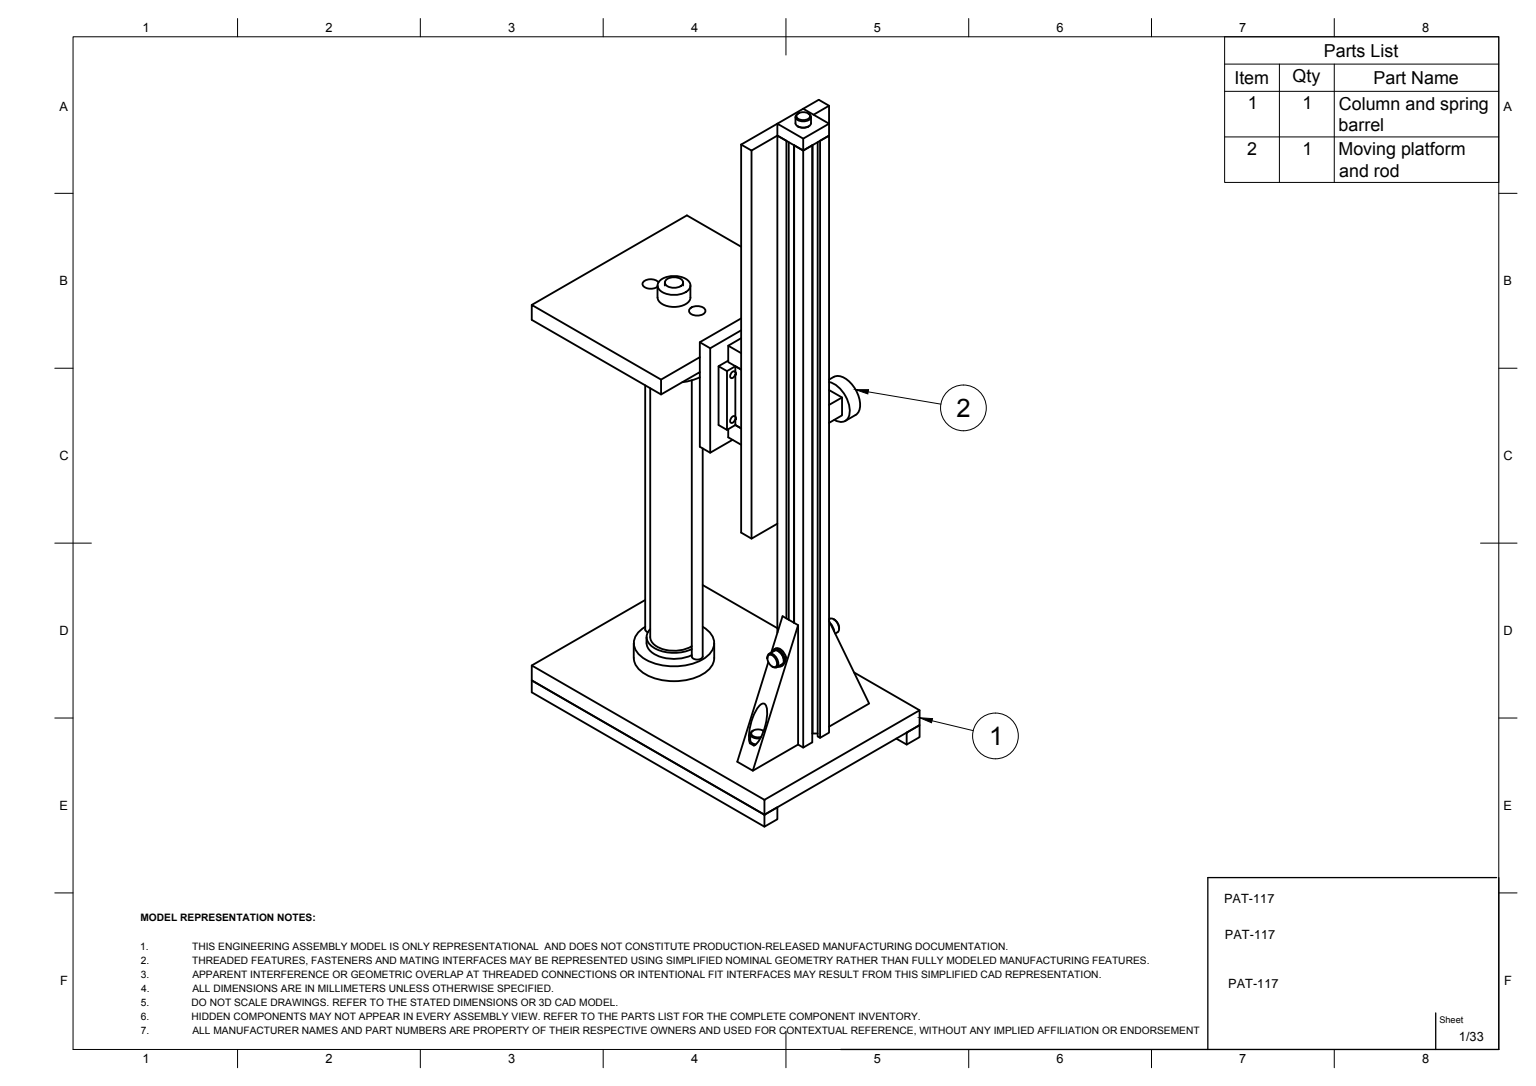
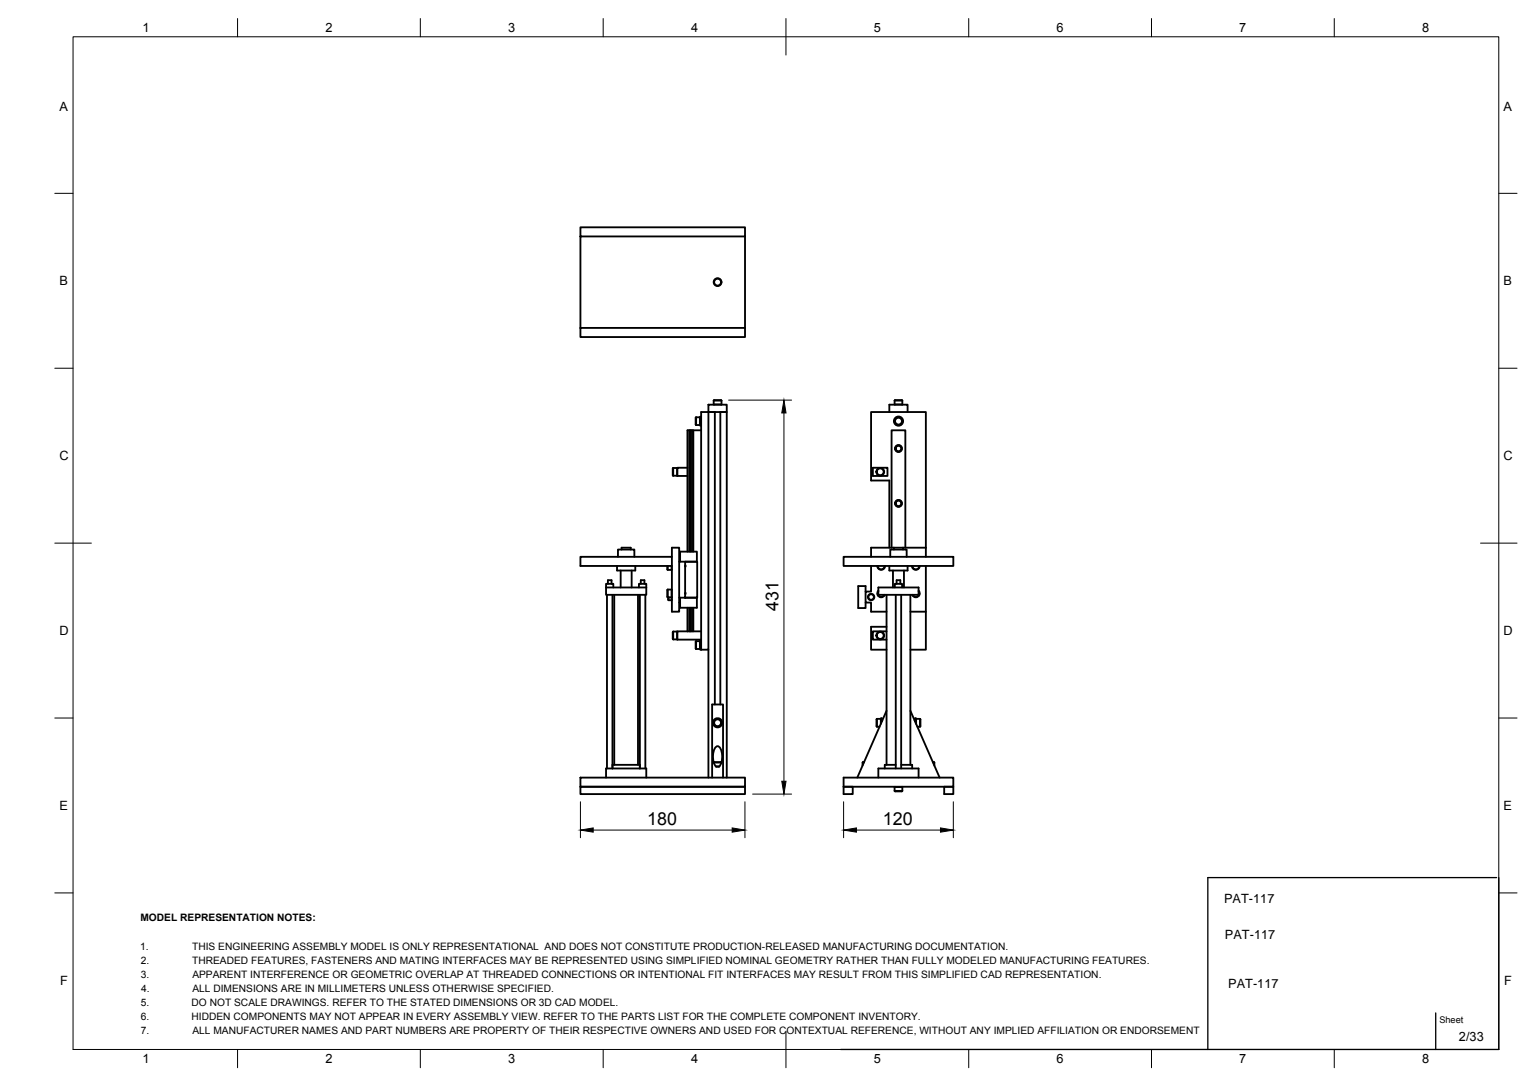
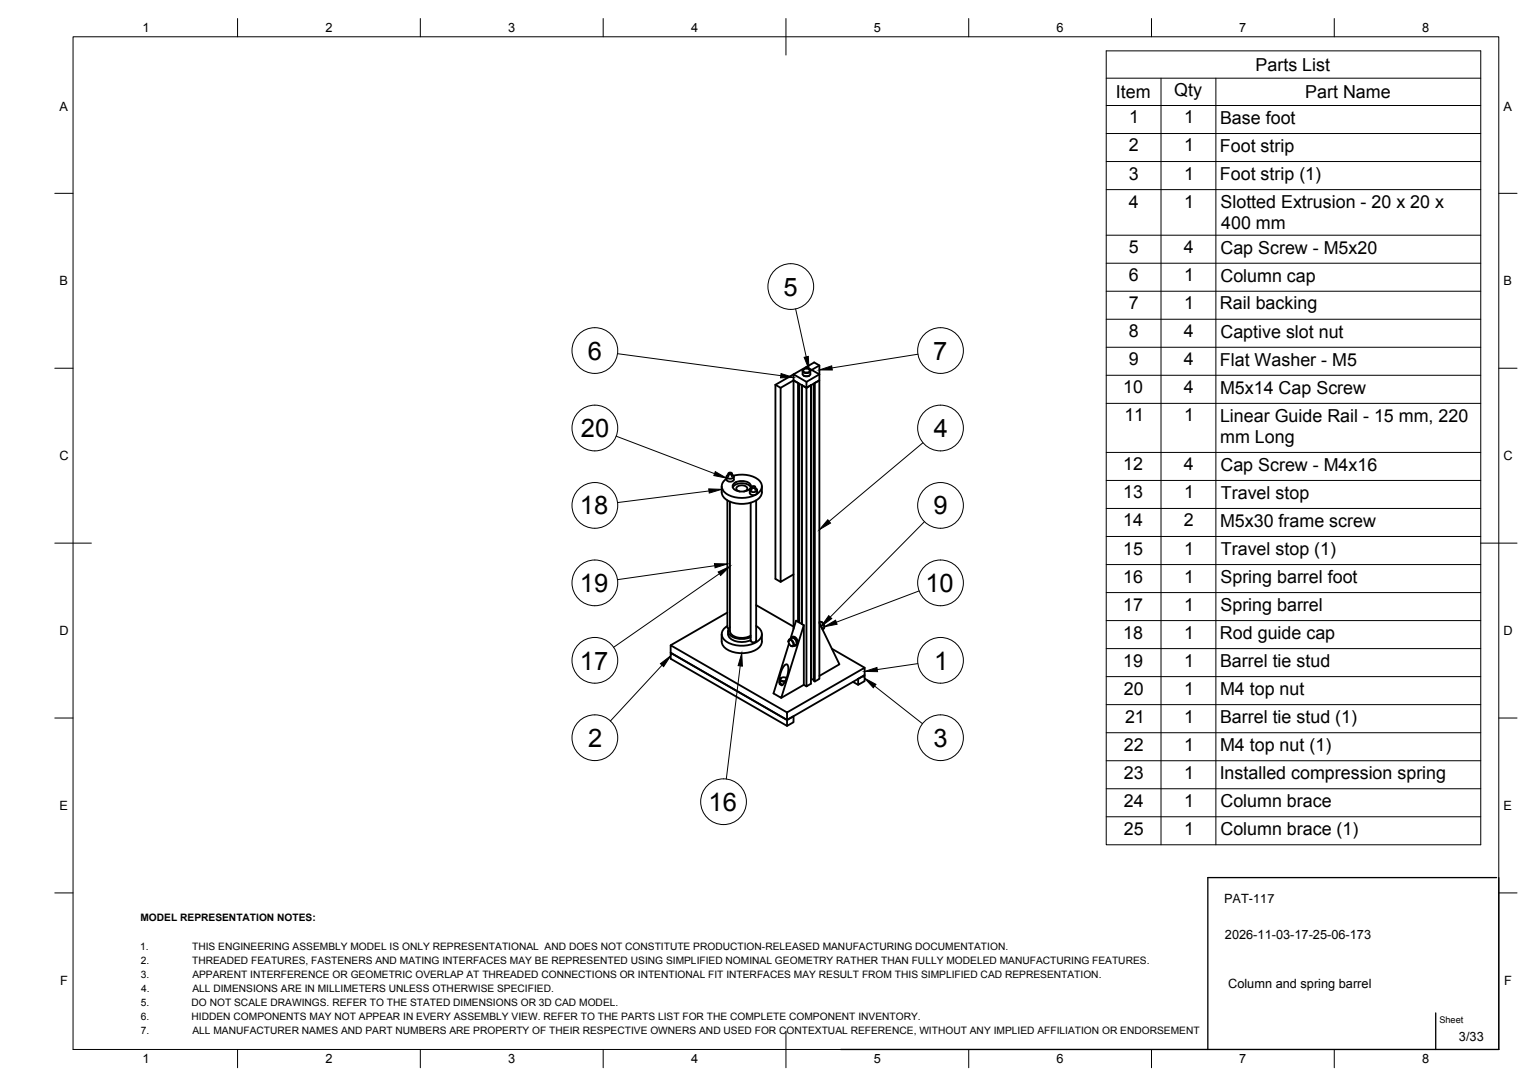
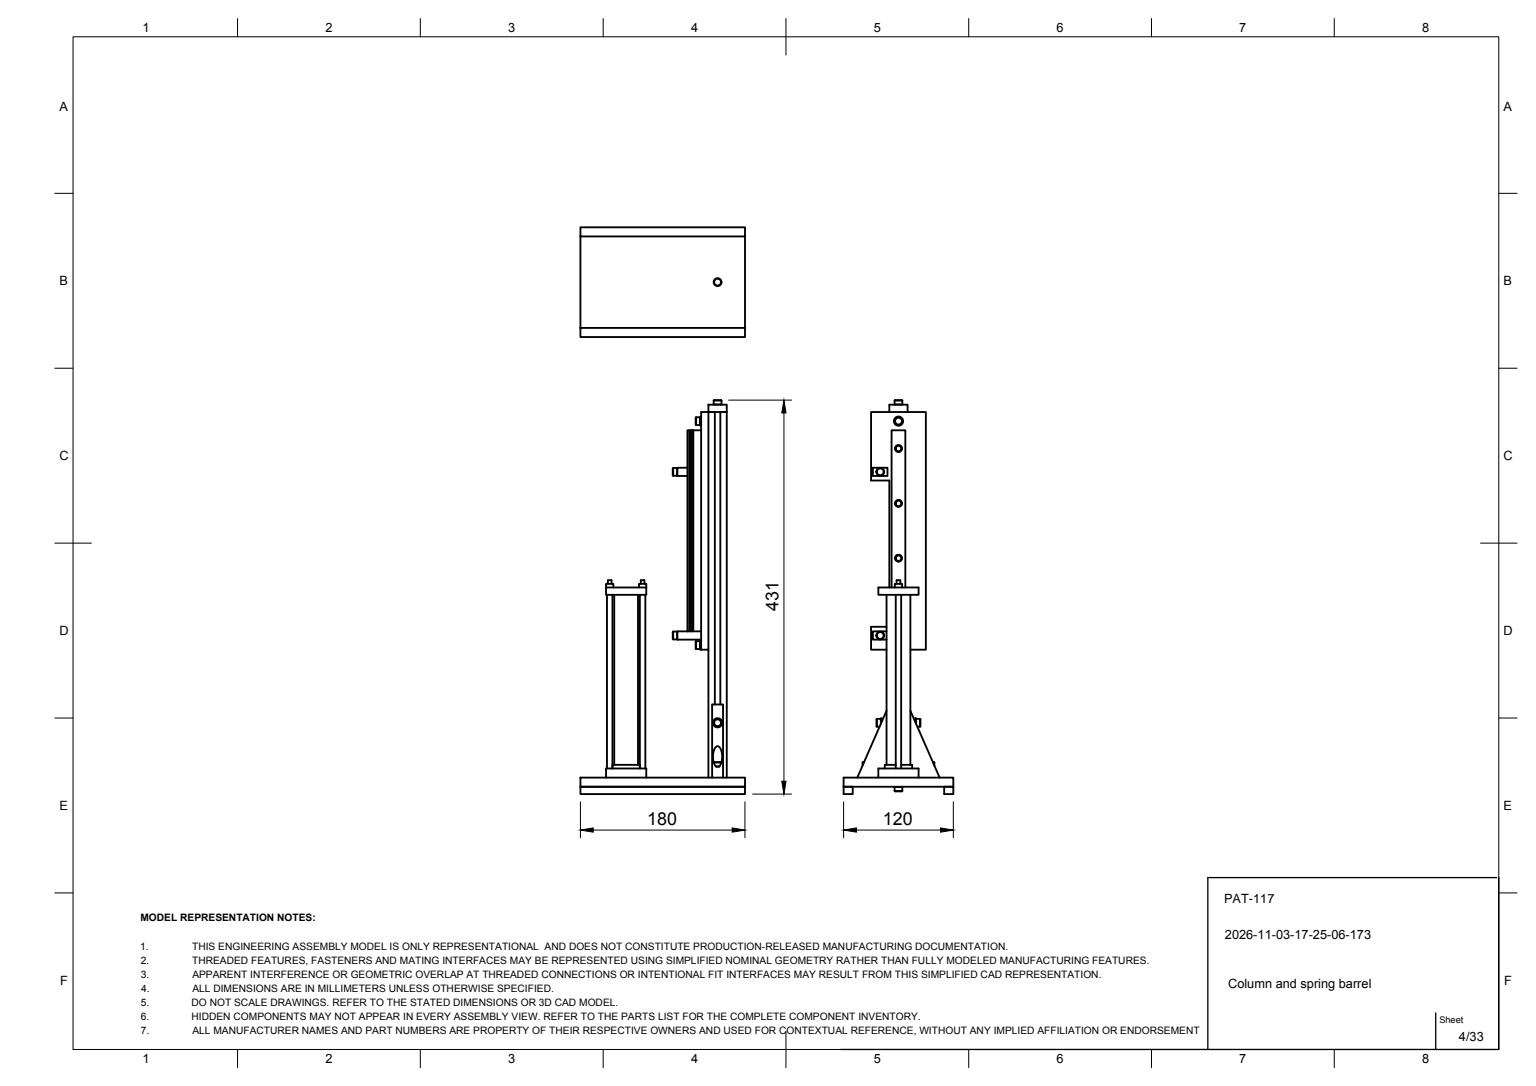
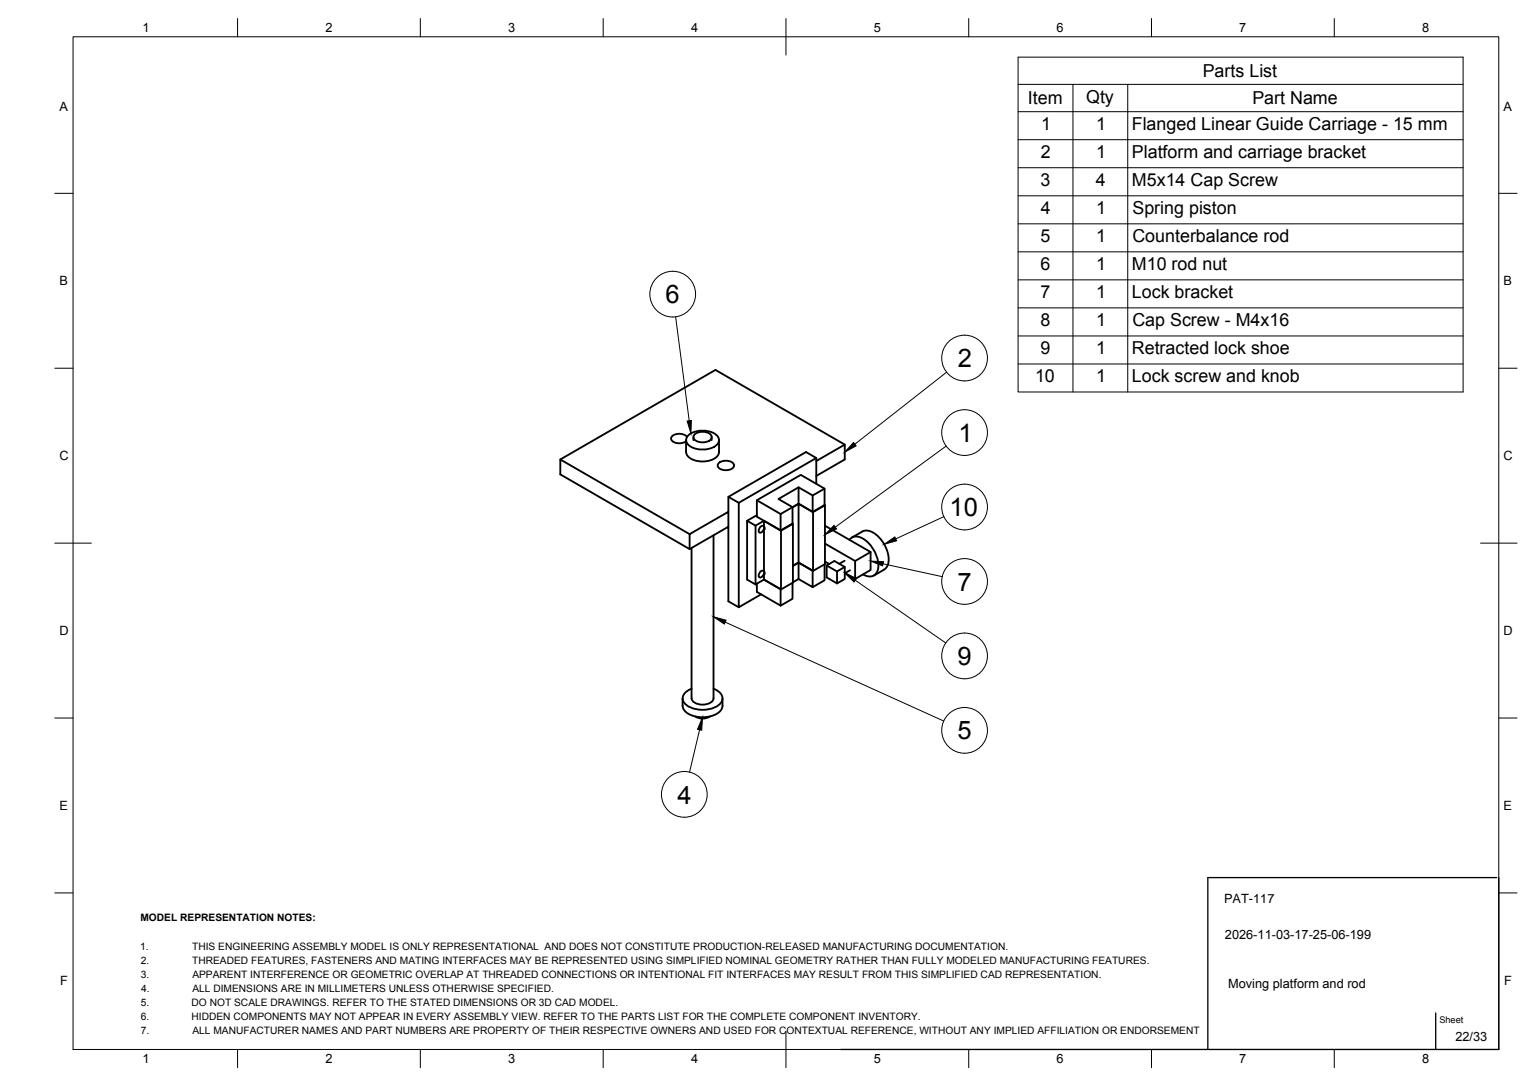
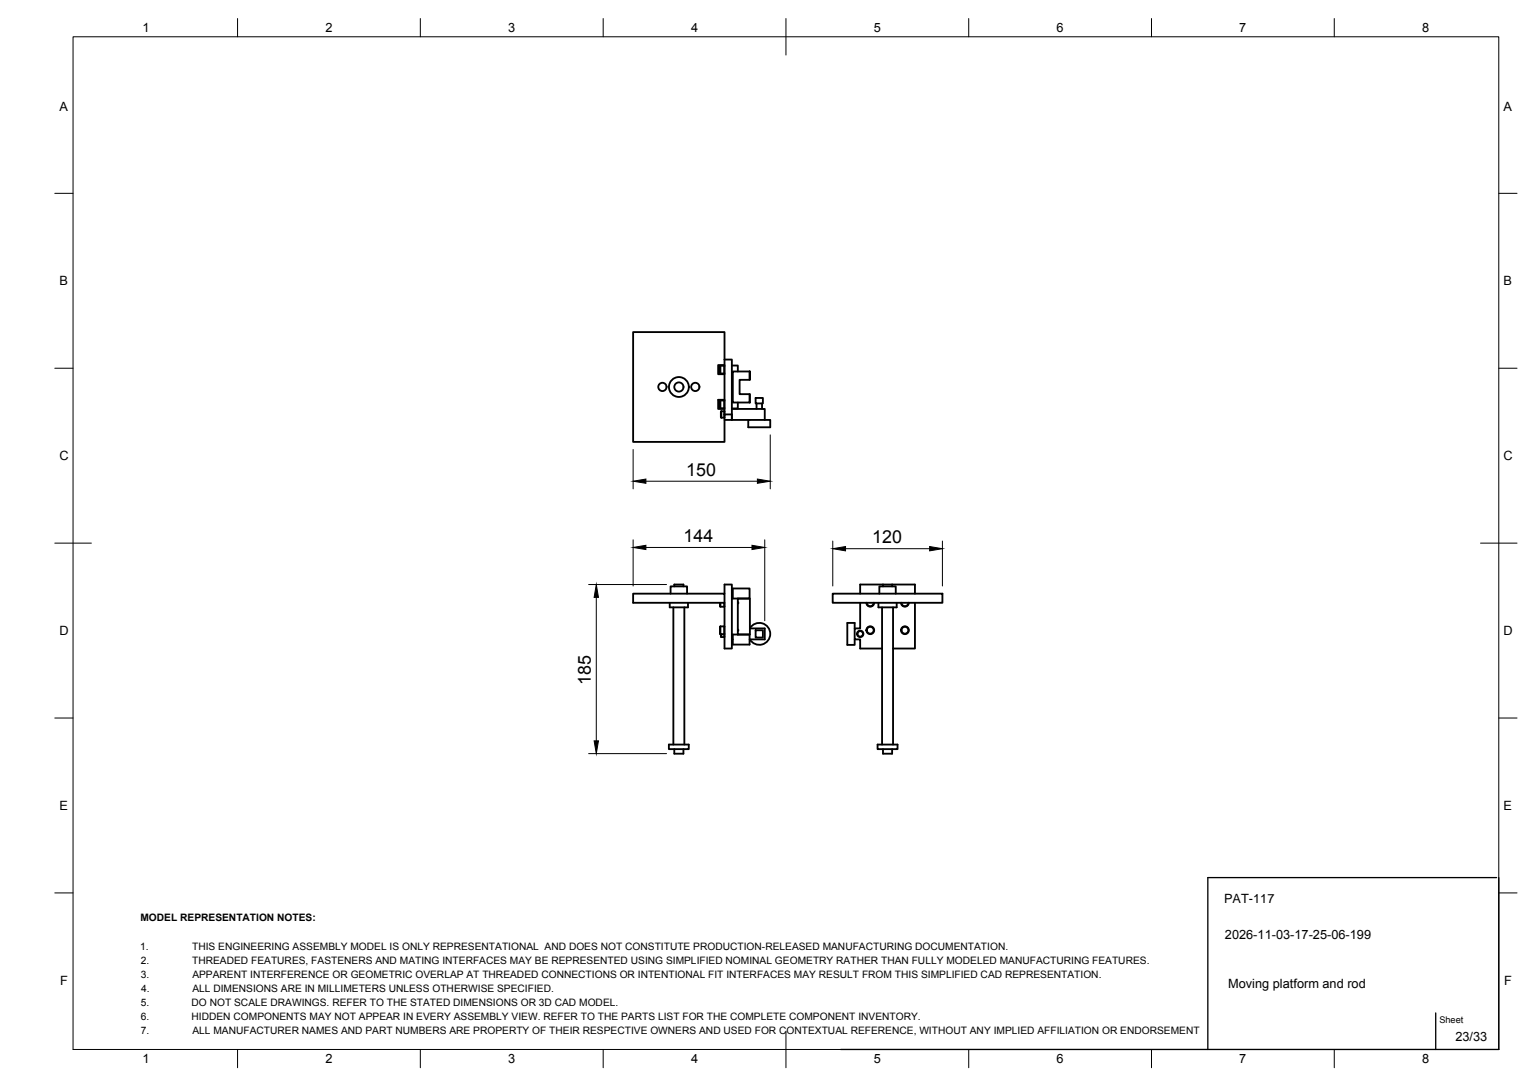
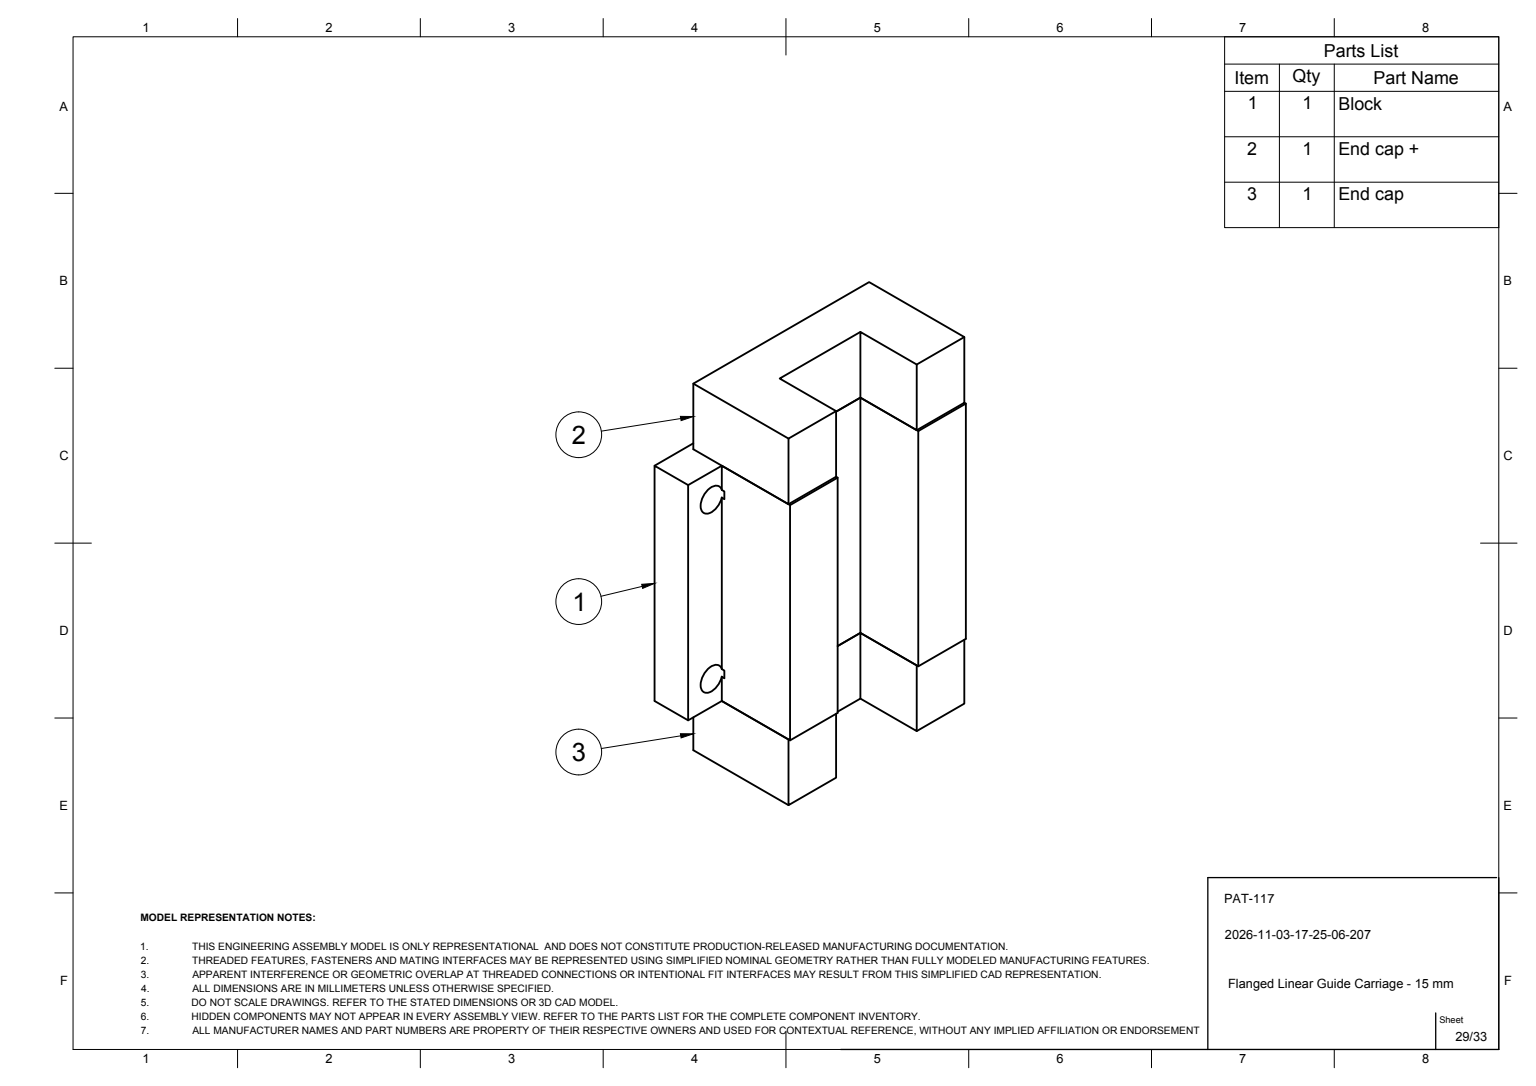
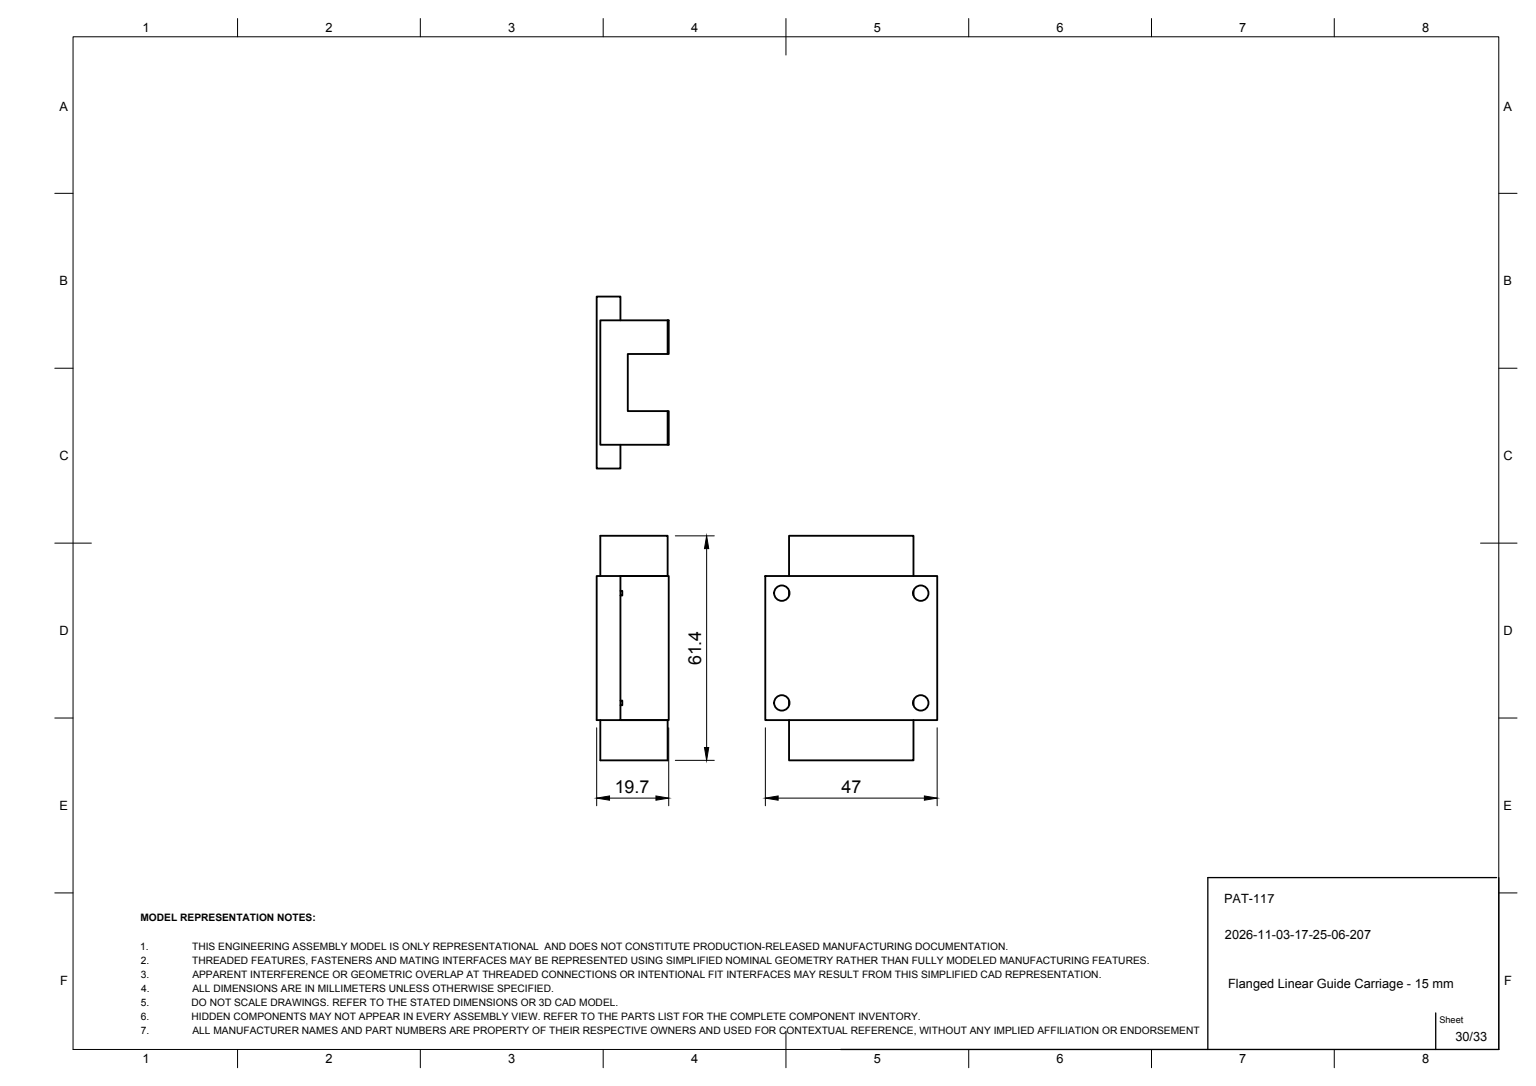
ISO-10303-21;
HEADER;
/* Generated by software containing ST-Developer
 * from STEP Tools, Inc. (www.steptools.com) 
 */

FILE_DESCRIPTION(
/* description */ ('Counterbalanced vertical column'),
/* implementation_level */ '2;1');

FILE_NAME(
/* name */ 'PAT-117',
/* time_stamp */ '2026-10-29T16:47:22-07:00',
/* author */ (''),
/* organization */ (''),
/* preprocessor_version */ 'ST-DEVELOPER v20.2',
/* originating_system */ 'Autodesk Translation Framework v15.17.0.0',
/* authorisation */ '');

FILE_SCHEMA (('AUTOMOTIVE_DESIGN { 1 0 10303 214 3 1 1 }'));
ENDSEC;

DATA;
#10=MECHANICAL_DESIGN_GEOMETRIC_PRESENTATION_REPRESENTATION('',(#350,#351,
#352,#353,#354,#355,#356,#357,#358,#359,#360,#361,#362,#363,#364,#365,#366,
#367,#368,#369,#370,#371,#372,#373,#374,#375,#376,#377,#378,#379,#380,#381,
#382,#383,#384),#15040);
#11=ITEM_DEFINED_TRANSFORMATION($,$,#8051,#8112);
#12=ITEM_DEFINED_TRANSFORMATION($,$,#8090,#8113);
#13=ITEM_DEFINED_TRANSFORMATION($,$,#8101,#8114);
#14=ITEM_DEFINED_TRANSFORMATION($,$,#7500,#8165);
#15=ITEM_DEFINED_TRANSFORMATION($,$,#7526,#8166);
#16=ITEM_DEFINED_TRANSFORMATION($,$,#7533,#8167);
#17=ITEM_DEFINED_TRANSFORMATION($,$,#7540,#8168);
#18=ITEM_DEFINED_TRANSFORMATION($,$,#7550,#8169);
#19=ITEM_DEFINED_TRANSFORMATION($,$,#7585,#8170);
#20=ITEM_DEFINED_TRANSFORMATION($,$,#7595,#8171);
#21=ITEM_DEFINED_TRANSFORMATION($,$,#7605,#8172);
#22=ITEM_DEFINED_TRANSFORMATION($,$,#7625,#8173);
#23=ITEM_DEFINED_TRANSFORMATION($,$,#7634,#8174);
#24=ITEM_DEFINED_TRANSFORMATION($,$,#7657,#8175);
#25=ITEM_DEFINED_TRANSFORMATION($,$,#7671,#8176);
#26=ITEM_DEFINED_TRANSFORMATION($,$,#7680,#8177);
#27=ITEM_DEFINED_TRANSFORMATION($,$,#7694,#8178);
#28=ITEM_DEFINED_TRANSFORMATION($,$,#7703,#8179);
#29=ITEM_DEFINED_TRANSFORMATION($,$,#7708,#8180);
#30=ITEM_DEFINED_TRANSFORMATION($,$,#7730,#8181);
#31=ITEM_DEFINED_TRANSFORMATION($,$,#7752,#8182);
#32=ITEM_DEFINED_TRANSFORMATION($,$,#7873,#8183);
#33=ITEM_DEFINED_TRANSFORMATION($,$,#7873,#8184);
#34=ITEM_DEFINED_TRANSFORMATION($,$,#7899,#8185);
#35=ITEM_DEFINED_TRANSFORMATION($,$,#7920,#8186);
#36=ITEM_DEFINED_TRANSFORMATION($,$,#8115,#8187);
#37=ITEM_DEFINED_TRANSFORMATION($,$,#7899,#8188);
#38=ITEM_DEFINED_TRANSFORMATION($,$,#7920,#8189);
#39=ITEM_DEFINED_TRANSFORMATION($,$,#8115,#8190);
#40=ITEM_DEFINED_TRANSFORMATION($,$,#7802,#8191);
#41=ITEM_DEFINED_TRANSFORMATION($,$,#8139,#8192);
#42=ITEM_DEFINED_TRANSFORMATION($,$,#8139,#8193);
#43=ITEM_DEFINED_TRANSFORMATION($,$,#8139,#8194);
#44=ITEM_DEFINED_TRANSFORMATION($,$,#8139,#8195);
#45=ITEM_DEFINED_TRANSFORMATION($,$,#7845,#8196);
#46=ITEM_DEFINED_TRANSFORMATION($,$,#7845,#8197);
#47=ITEM_DEFINED_TRANSFORMATION($,$,#7873,#8198);
#48=ITEM_DEFINED_TRANSFORMATION($,$,#7899,#8199);
#49=ITEM_DEFINED_TRANSFORMATION($,$,#7920,#8200);
#50=ITEM_DEFINED_TRANSFORMATION($,$,#8115,#8201);
#51=ITEM_DEFINED_TRANSFORMATION($,$,#7873,#8202);
#52=ITEM_DEFINED_TRANSFORMATION($,$,#7899,#8203);
#53=ITEM_DEFINED_TRANSFORMATION($,$,#7920,#8204);
#54=ITEM_DEFINED_TRANSFORMATION($,$,#8115,#8205);
#55=ITEM_DEFINED_TRANSFORMATION($,$,#7932,#8206);
#56=ITEM_DEFINED_TRANSFORMATION($,$,#7983,#8207);
#57=ITEM_DEFINED_TRANSFORMATION($,$,#7992,#8208);
#58=ITEM_DEFINED_TRANSFORMATION($,$,#8010,#8209);
#59=ITEM_DEFINED_TRANSFORMATION($,$,#8019,#8210);
#60=ITEM_DEFINED_TRANSFORMATION($,$,#8033,#8211);
#61=ITEM_DEFINED_TRANSFORMATION($,$,#8040,#8212);
#62=ITEM_DEFINED_TRANSFORMATION($,$,#8050,#8213);
#63=ITEM_DEFINED_TRANSFORMATION($,$,#8115,#8214);
#64=ITEM_DEFINED_TRANSFORMATION($,$,#8115,#8215);
#65=ITEM_DEFINED_TRANSFORMATION($,$,#8115,#8216);
#66=ITEM_DEFINED_TRANSFORMATION($,$,#8115,#8217);
#67=ITEM_DEFINED_TRANSFORMATION($,$,#8139,#8218);
#68=ITEM_DEFINED_TRANSFORMATION($,$,#7499,#8219);
#69=ITEM_DEFINED_TRANSFORMATION($,$,#7931,#8220);
#70=(
REPRESENTATION_RELATIONSHIP($,$,#15216,#15215)
REPRESENTATION_RELATIONSHIP_WITH_TRANSFORMATION(#11)
SHAPE_REPRESENTATION_RELATIONSHIP()
);
#71=(
REPRESENTATION_RELATIONSHIP($,$,#15217,#15215)
REPRESENTATION_RELATIONSHIP_WITH_TRANSFORMATION(#12)
SHAPE_REPRESENTATION_RELATIONSHIP()
);
#72=(
REPRESENTATION_RELATIONSHIP($,$,#15218,#15215)
REPRESENTATION_RELATIONSHIP_WITH_TRANSFORMATION(#13)
SHAPE_REPRESENTATION_RELATIONSHIP()
);
#73=(
REPRESENTATION_RELATIONSHIP($,$,#15184,#15183)
REPRESENTATION_RELATIONSHIP_WITH_TRANSFORMATION(#14)
SHAPE_REPRESENTATION_RELATIONSHIP()
);
#74=(
REPRESENTATION_RELATIONSHIP($,$,#15185,#15183)
REPRESENTATION_RELATIONSHIP_WITH_TRANSFORMATION(#15)
SHAPE_REPRESENTATION_RELATIONSHIP()
);
#75=(
REPRESENTATION_RELATIONSHIP($,$,#15186,#15183)
REPRESENTATION_RELATIONSHIP_WITH_TRANSFORMATION(#16)
SHAPE_REPRESENTATION_RELATIONSHIP()
);
#76=(
REPRESENTATION_RELATIONSHIP($,$,#15187,#15183)
REPRESENTATION_RELATIONSHIP_WITH_TRANSFORMATION(#17)
SHAPE_REPRESENTATION_RELATIONSHIP()
);
#77=(
REPRESENTATION_RELATIONSHIP($,$,#15188,#15183)
REPRESENTATION_RELATIONSHIP_WITH_TRANSFORMATION(#18)
SHAPE_REPRESENTATION_RELATIONSHIP()
);
#78=(
REPRESENTATION_RELATIONSHIP($,$,#15189,#15183)
REPRESENTATION_RELATIONSHIP_WITH_TRANSFORMATION(#19)
SHAPE_REPRESENTATION_RELATIONSHIP()
);
#79=(
REPRESENTATION_RELATIONSHIP($,$,#15190,#15183)
REPRESENTATION_RELATIONSHIP_WITH_TRANSFORMATION(#20)
SHAPE_REPRESENTATION_RELATIONSHIP()
);
#80=(
REPRESENTATION_RELATIONSHIP($,$,#15191,#15183)
REPRESENTATION_RELATIONSHIP_WITH_TRANSFORMATION(#21)
SHAPE_REPRESENTATION_RELATIONSHIP()
);
#81=(
REPRESENTATION_RELATIONSHIP($,$,#15192,#15183)
REPRESENTATION_RELATIONSHIP_WITH_TRANSFORMATION(#22)
SHAPE_REPRESENTATION_RELATIONSHIP()
);
#82=(
REPRESENTATION_RELATIONSHIP($,$,#15193,#15183)
REPRESENTATION_RELATIONSHIP_WITH_TRANSFORMATION(#23)
SHAPE_REPRESENTATION_RELATIONSHIP()
);
#83=(
REPRESENTATION_RELATIONSHIP($,$,#15194,#15183)
REPRESENTATION_RELATIONSHIP_WITH_TRANSFORMATION(#24)
SHAPE_REPRESENTATION_RELATIONSHIP()
);
#84=(
REPRESENTATION_RELATIONSHIP($,$,#15195,#15183)
REPRESENTATION_RELATIONSHIP_WITH_TRANSFORMATION(#25)
SHAPE_REPRESENTATION_RELATIONSHIP()
);
#85=(
REPRESENTATION_RELATIONSHIP($,$,#15196,#15183)
REPRESENTATION_RELATIONSHIP_WITH_TRANSFORMATION(#26)
SHAPE_REPRESENTATION_RELATIONSHIP()
);
#86=(
REPRESENTATION_RELATIONSHIP($,$,#15197,#15183)
REPRESENTATION_RELATIONSHIP_WITH_TRANSFORMATION(#27)
SHAPE_REPRESENTATION_RELATIONSHIP()
);
#87=(
REPRESENTATION_RELATIONSHIP($,$,#15198,#15183)
REPRESENTATION_RELATIONSHIP_WITH_TRANSFORMATION(#28)
SHAPE_REPRESENTATION_RELATIONSHIP()
);
#88=(
REPRESENTATION_RELATIONSHIP($,$,#15199,#15183)
REPRESENTATION_RELATIONSHIP_WITH_TRANSFORMATION(#29)
SHAPE_REPRESENTATION_RELATIONSHIP()
);
#89=(
REPRESENTATION_RELATIONSHIP($,$,#15200,#15183)
REPRESENTATION_RELATIONSHIP_WITH_TRANSFORMATION(#30)
SHAPE_REPRESENTATION_RELATIONSHIP()
);
#90=(
REPRESENTATION_RELATIONSHIP($,$,#15201,#15183)
REPRESENTATION_RELATIONSHIP_WITH_TRANSFORMATION(#31)
SHAPE_REPRESENTATION_RELATIONSHIP()
);
#91=(
REPRESENTATION_RELATIONSHIP($,$,#15204,#15183)
REPRESENTATION_RELATIONSHIP_WITH_TRANSFORMATION(#32)
SHAPE_REPRESENTATION_RELATIONSHIP()
);
#92=(
REPRESENTATION_RELATIONSHIP($,$,#15204,#15183)
REPRESENTATION_RELATIONSHIP_WITH_TRANSFORMATION(#33)
SHAPE_REPRESENTATION_RELATIONSHIP()
);
#93=(
REPRESENTATION_RELATIONSHIP($,$,#15205,#15183)
REPRESENTATION_RELATIONSHIP_WITH_TRANSFORMATION(#34)
SHAPE_REPRESENTATION_RELATIONSHIP()
);
#94=(
REPRESENTATION_RELATIONSHIP($,$,#15206,#15183)
REPRESENTATION_RELATIONSHIP_WITH_TRANSFORMATION(#35)
SHAPE_REPRESENTATION_RELATIONSHIP()
);
#95=(
REPRESENTATION_RELATIONSHIP($,$,#15219,#15183)
REPRESENTATION_RELATIONSHIP_WITH_TRANSFORMATION(#36)
SHAPE_REPRESENTATION_RELATIONSHIP()
);
#96=(
REPRESENTATION_RELATIONSHIP($,$,#15205,#15183)
REPRESENTATION_RELATIONSHIP_WITH_TRANSFORMATION(#37)
SHAPE_REPRESENTATION_RELATIONSHIP()
);
#97=(
REPRESENTATION_RELATIONSHIP($,$,#15206,#15183)
REPRESENTATION_RELATIONSHIP_WITH_TRANSFORMATION(#38)
SHAPE_REPRESENTATION_RELATIONSHIP()
);
#98=(
REPRESENTATION_RELATIONSHIP($,$,#15219,#15183)
REPRESENTATION_RELATIONSHIP_WITH_TRANSFORMATION(#39)
SHAPE_REPRESENTATION_RELATIONSHIP()
);
#99=(
REPRESENTATION_RELATIONSHIP($,$,#15202,#15183)
REPRESENTATION_RELATIONSHIP_WITH_TRANSFORMATION(#40)
SHAPE_REPRESENTATION_RELATIONSHIP()
);
#100=(
REPRESENTATION_RELATIONSHIP($,$,#15220,#15183)
REPRESENTATION_RELATIONSHIP_WITH_TRANSFORMATION(#41)
SHAPE_REPRESENTATION_RELATIONSHIP()
);
#101=(
REPRESENTATION_RELATIONSHIP($,$,#15220,#15183)
REPRESENTATION_RELATIONSHIP_WITH_TRANSFORMATION(#42)
SHAPE_REPRESENTATION_RELATIONSHIP()
);
#102=(
REPRESENTATION_RELATIONSHIP($,$,#15220,#15183)
REPRESENTATION_RELATIONSHIP_WITH_TRANSFORMATION(#43)
SHAPE_REPRESENTATION_RELATIONSHIP()
);
#103=(
REPRESENTATION_RELATIONSHIP($,$,#15220,#15183)
REPRESENTATION_RELATIONSHIP_WITH_TRANSFORMATION(#44)
SHAPE_REPRESENTATION_RELATIONSHIP()
);
#104=(
REPRESENTATION_RELATIONSHIP($,$,#15203,#15183)
REPRESENTATION_RELATIONSHIP_WITH_TRANSFORMATION(#45)
SHAPE_REPRESENTATION_RELATIONSHIP()
);
#105=(
REPRESENTATION_RELATIONSHIP($,$,#15203,#15183)
REPRESENTATION_RELATIONSHIP_WITH_TRANSFORMATION(#46)
SHAPE_REPRESENTATION_RELATIONSHIP()
);
#106=(
REPRESENTATION_RELATIONSHIP($,$,#15204,#15183)
REPRESENTATION_RELATIONSHIP_WITH_TRANSFORMATION(#47)
SHAPE_REPRESENTATION_RELATIONSHIP()
);
#107=(
REPRESENTATION_RELATIONSHIP($,$,#15205,#15183)
REPRESENTATION_RELATIONSHIP_WITH_TRANSFORMATION(#48)
SHAPE_REPRESENTATION_RELATIONSHIP()
);
#108=(
REPRESENTATION_RELATIONSHIP($,$,#15206,#15183)
REPRESENTATION_RELATIONSHIP_WITH_TRANSFORMATION(#49)
SHAPE_REPRESENTATION_RELATIONSHIP()
);
#109=(
REPRESENTATION_RELATIONSHIP($,$,#15219,#15183)
REPRESENTATION_RELATIONSHIP_WITH_TRANSFORMATION(#50)
SHAPE_REPRESENTATION_RELATIONSHIP()
);
#110=(
REPRESENTATION_RELATIONSHIP($,$,#15204,#15183)
REPRESENTATION_RELATIONSHIP_WITH_TRANSFORMATION(#51)
SHAPE_REPRESENTATION_RELATIONSHIP()
);
#111=(
REPRESENTATION_RELATIONSHIP($,$,#15205,#15183)
REPRESENTATION_RELATIONSHIP_WITH_TRANSFORMATION(#52)
SHAPE_REPRESENTATION_RELATIONSHIP()
);
#112=(
REPRESENTATION_RELATIONSHIP($,$,#15206,#15183)
REPRESENTATION_RELATIONSHIP_WITH_TRANSFORMATION(#53)
SHAPE_REPRESENTATION_RELATIONSHIP()
);
#113=(
REPRESENTATION_RELATIONSHIP($,$,#15219,#15183)
REPRESENTATION_RELATIONSHIP_WITH_TRANSFORMATION(#54)
SHAPE_REPRESENTATION_RELATIONSHIP()
);
#114=(
REPRESENTATION_RELATIONSHIP($,$,#15208,#15207)
REPRESENTATION_RELATIONSHIP_WITH_TRANSFORMATION(#55)
SHAPE_REPRESENTATION_RELATIONSHIP()
);
#115=(
REPRESENTATION_RELATIONSHIP($,$,#15209,#15207)
REPRESENTATION_RELATIONSHIP_WITH_TRANSFORMATION(#56)
SHAPE_REPRESENTATION_RELATIONSHIP()
);
#116=(
REPRESENTATION_RELATIONSHIP($,$,#15210,#15207)
REPRESENTATION_RELATIONSHIP_WITH_TRANSFORMATION(#57)
SHAPE_REPRESENTATION_RELATIONSHIP()
);
#117=(
REPRESENTATION_RELATIONSHIP($,$,#15211,#15207)
REPRESENTATION_RELATIONSHIP_WITH_TRANSFORMATION(#58)
SHAPE_REPRESENTATION_RELATIONSHIP()
);
#118=(
REPRESENTATION_RELATIONSHIP($,$,#15212,#15207)
REPRESENTATION_RELATIONSHIP_WITH_TRANSFORMATION(#59)
SHAPE_REPRESENTATION_RELATIONSHIP()
);
#119=(
REPRESENTATION_RELATIONSHIP($,$,#15213,#15207)
REPRESENTATION_RELATIONSHIP_WITH_TRANSFORMATION(#60)
SHAPE_REPRESENTATION_RELATIONSHIP()
);
#120=(
REPRESENTATION_RELATIONSHIP($,$,#15214,#15207)
REPRESENTATION_RELATIONSHIP_WITH_TRANSFORMATION(#61)
SHAPE_REPRESENTATION_RELATIONSHIP()
);
#121=(
REPRESENTATION_RELATIONSHIP($,$,#15215,#15207)
REPRESENTATION_RELATIONSHIP_WITH_TRANSFORMATION(#62)
SHAPE_REPRESENTATION_RELATIONSHIP()
);
#122=(
REPRESENTATION_RELATIONSHIP($,$,#15219,#15207)
REPRESENTATION_RELATIONSHIP_WITH_TRANSFORMATION(#63)
SHAPE_REPRESENTATION_RELATIONSHIP()
);
#123=(
REPRESENTATION_RELATIONSHIP($,$,#15219,#15207)
REPRESENTATION_RELATIONSHIP_WITH_TRANSFORMATION(#64)
SHAPE_REPRESENTATION_RELATIONSHIP()
);
#124=(
REPRESENTATION_RELATIONSHIP($,$,#15219,#15207)
REPRESENTATION_RELATIONSHIP_WITH_TRANSFORMATION(#65)
SHAPE_REPRESENTATION_RELATIONSHIP()
);
#125=(
REPRESENTATION_RELATIONSHIP($,$,#15219,#15207)
REPRESENTATION_RELATIONSHIP_WITH_TRANSFORMATION(#66)
SHAPE_REPRESENTATION_RELATIONSHIP()
);
#126=(
REPRESENTATION_RELATIONSHIP($,$,#15220,#15207)
REPRESENTATION_RELATIONSHIP_WITH_TRANSFORMATION(#67)
SHAPE_REPRESENTATION_RELATIONSHIP()
);
#127=(
REPRESENTATION_RELATIONSHIP($,$,#15183,#15182)
REPRESENTATION_RELATIONSHIP_WITH_TRANSFORMATION(#68)
SHAPE_REPRESENTATION_RELATIONSHIP()
);
#128=(
REPRESENTATION_RELATIONSHIP($,$,#15207,#15182)
REPRESENTATION_RELATIONSHIP_WITH_TRANSFORMATION(#69)
SHAPE_REPRESENTATION_RELATIONSHIP()
);
#129=CONTEXT_DEPENDENT_SHAPE_REPRESENTATION(#70,#15121);
#130=CONTEXT_DEPENDENT_SHAPE_REPRESENTATION(#71,#15122);
#131=CONTEXT_DEPENDENT_SHAPE_REPRESENTATION(#72,#15123);
#132=CONTEXT_DEPENDENT_SHAPE_REPRESENTATION(#73,#15126);
#133=CONTEXT_DEPENDENT_SHAPE_REPRESENTATION(#74,#15127);
#134=CONTEXT_DEPENDENT_SHAPE_REPRESENTATION(#75,#15128);
#135=CONTEXT_DEPENDENT_SHAPE_REPRESENTATION(#76,#15129);
#136=CONTEXT_DEPENDENT_SHAPE_REPRESENTATION(#77,#15130);
#137=CONTEXT_DEPENDENT_SHAPE_REPRESENTATION(#78,#15131);
#138=CONTEXT_DEPENDENT_SHAPE_REPRESENTATION(#79,#15132);
#139=CONTEXT_DEPENDENT_SHAPE_REPRESENTATION(#80,#15133);
#140=CONTEXT_DEPENDENT_SHAPE_REPRESENTATION(#81,#15134);
#141=CONTEXT_DEPENDENT_SHAPE_REPRESENTATION(#82,#15135);
#142=CONTEXT_DEPENDENT_SHAPE_REPRESENTATION(#83,#15136);
#143=CONTEXT_DEPENDENT_SHAPE_REPRESENTATION(#84,#15137);
#144=CONTEXT_DEPENDENT_SHAPE_REPRESENTATION(#85,#15138);
#145=CONTEXT_DEPENDENT_SHAPE_REPRESENTATION(#86,#15139);
#146=CONTEXT_DEPENDENT_SHAPE_REPRESENTATION(#87,#15140);
#147=CONTEXT_DEPENDENT_SHAPE_REPRESENTATION(#88,#15141);
#148=CONTEXT_DEPENDENT_SHAPE_REPRESENTATION(#89,#15142);
#149=CONTEXT_DEPENDENT_SHAPE_REPRESENTATION(#90,#15143);
#150=CONTEXT_DEPENDENT_SHAPE_REPRESENTATION(#91,#15144);
#151=CONTEXT_DEPENDENT_SHAPE_REPRESENTATION(#92,#15145);
#152=CONTEXT_DEPENDENT_SHAPE_REPRESENTATION(#93,#15146);
#153=CONTEXT_DEPENDENT_SHAPE_REPRESENTATION(#94,#15147);
#154=CONTEXT_DEPENDENT_SHAPE_REPRESENTATION(#95,#15148);
#155=CONTEXT_DEPENDENT_SHAPE_REPRESENTATION(#96,#15149);
#156=CONTEXT_DEPENDENT_SHAPE_REPRESENTATION(#97,#15150);
#157=CONTEXT_DEPENDENT_SHAPE_REPRESENTATION(#98,#15151);
#158=CONTEXT_DEPENDENT_SHAPE_REPRESENTATION(#99,#15152);
#159=CONTEXT_DEPENDENT_SHAPE_REPRESENTATION(#100,#15153);
#160=CONTEXT_DEPENDENT_SHAPE_REPRESENTATION(#101,#15154);
#161=CONTEXT_DEPENDENT_SHAPE_REPRESENTATION(#102,#15155);
#162=CONTEXT_DEPENDENT_SHAPE_REPRESENTATION(#103,#15156);
#163=CONTEXT_DEPENDENT_SHAPE_REPRESENTATION(#104,#15157);
#164=CONTEXT_DEPENDENT_SHAPE_REPRESENTATION(#105,#15158);
#165=CONTEXT_DEPENDENT_SHAPE_REPRESENTATION(#106,#15159);
#166=CONTEXT_DEPENDENT_SHAPE_REPRESENTATION(#107,#15160);
#167=CONTEXT_DEPENDENT_SHAPE_REPRESENTATION(#108,#15161);
#168=CONTEXT_DEPENDENT_SHAPE_REPRESENTATION(#109,#15162);
#169=CONTEXT_DEPENDENT_SHAPE_REPRESENTATION(#110,#15163);
#170=CONTEXT_DEPENDENT_SHAPE_REPRESENTATION(#111,#15164);
#171=CONTEXT_DEPENDENT_SHAPE_REPRESENTATION(#112,#15165);
#172=CONTEXT_DEPENDENT_SHAPE_REPRESENTATION(#113,#15166);
#173=CONTEXT_DEPENDENT_SHAPE_REPRESENTATION(#114,#15167);
#174=CONTEXT_DEPENDENT_SHAPE_REPRESENTATION(#115,#15168);
#175=CONTEXT_DEPENDENT_SHAPE_REPRESENTATION(#116,#15169);
#176=CONTEXT_DEPENDENT_SHAPE_REPRESENTATION(#117,#15170);
#177=CONTEXT_DEPENDENT_SHAPE_REPRESENTATION(#118,#15171);
#178=CONTEXT_DEPENDENT_SHAPE_REPRESENTATION(#119,#15172);
#179=CONTEXT_DEPENDENT_SHAPE_REPRESENTATION(#120,#15173);
#180=CONTEXT_DEPENDENT_SHAPE_REPRESENTATION(#121,#15174);
#181=CONTEXT_DEPENDENT_SHAPE_REPRESENTATION(#122,#15175);
#182=CONTEXT_DEPENDENT_SHAPE_REPRESENTATION(#123,#15176);
#183=CONTEXT_DEPENDENT_SHAPE_REPRESENTATION(#124,#15177);
#184=CONTEXT_DEPENDENT_SHAPE_REPRESENTATION(#125,#15178);
#185=CONTEXT_DEPENDENT_SHAPE_REPRESENTATION(#126,#15179);
#186=CONTEXT_DEPENDENT_SHAPE_REPRESENTATION(#127,#15180);
#187=CONTEXT_DEPENDENT_SHAPE_REPRESENTATION(#128,#15181);
#188=NEXT_ASSEMBLY_USAGE_OCCURRENCE('Block:1','Block:1','Block:1',#15255,
#15256,'Block:1');
#189=NEXT_ASSEMBLY_USAGE_OCCURRENCE('End cap +:1','End cap +:1',
'End cap +:1',#15255,#15257,'End cap +:1');
#190=NEXT_ASSEMBLY_USAGE_OCCURRENCE('End cap:1','End cap:1','End cap:1',
#15255,#15258,'End cap:1');
#191=NEXT_ASSEMBLY_USAGE_OCCURRENCE('Base foot:1','Base foot:1',
'Base foot:1',#15223,#15224,'Base foot:1');
#192=NEXT_ASSEMBLY_USAGE_OCCURRENCE('Foot strip:1','Foot strip:1',
'Foot strip:1',#15223,#15225,'Foot strip:1');
#193=NEXT_ASSEMBLY_USAGE_OCCURRENCE('Foot strip (1):1',
'Foot strip (1):1','Foot strip (1):1',#15223,#15226,'Foot strip (1):1');
#194=NEXT_ASSEMBLY_USAGE_OCCURRENCE('Column cap:1','Column cap:1',
'Column cap:1',#15223,#15227,'Column cap:1');
#195=NEXT_ASSEMBLY_USAGE_OCCURRENCE('Rail backing:1','Rail backing:1',
'Rail backing:1',#15223,#15228,'Rail backing:1');
#196=NEXT_ASSEMBLY_USAGE_OCCURRENCE('Travel stop:1','Travel stop:1',
'Travel stop:1',#15223,#15229,'Travel stop:1');
#197=NEXT_ASSEMBLY_USAGE_OCCURRENCE('Travel stop (1):1',
'Travel stop (1):1','Travel stop (1):1',#15223,#15230,
'Travel stop (1):1');
#198=NEXT_ASSEMBLY_USAGE_OCCURRENCE('Spring barrel foot:1',
'Spring barrel foot:1','Spring barrel foot:1',#15223,#15231,
'Spring barrel foot:1');
#199=NEXT_ASSEMBLY_USAGE_OCCURRENCE('Spring barrel:1','Spring barrel:1',
'Spring barrel:1',#15223,#15232,'Spring barrel:1');
#200=NEXT_ASSEMBLY_USAGE_OCCURRENCE('Rod guide cap:1','Rod guide cap:1',
'Rod guide cap:1',#15223,#15233,'Rod guide cap:1');
#201=NEXT_ASSEMBLY_USAGE_OCCURRENCE('Barrel tie stud:1',
'Barrel tie stud:1','Barrel tie stud:1',#15223,#15234,
'Barrel tie stud:1');
#202=NEXT_ASSEMBLY_USAGE_OCCURRENCE('M4 top nut:1','M4 top nut:1',
'M4 top nut:1',#15223,#15235,'M4 top nut:1');
#203=NEXT_ASSEMBLY_USAGE_OCCURRENCE('Barrel tie stud (1):1',
'Barrel tie stud (1):1','Barrel tie stud (1):1',#15223,#15236,
'Barrel tie stud (1):1');
#204=NEXT_ASSEMBLY_USAGE_OCCURRENCE('M4 top nut (1):1',
'M4 top nut (1):1','M4 top nut (1):1',#15223,#15237,'M4 top nut (1):1');
#205=NEXT_ASSEMBLY_USAGE_OCCURRENCE('Installed compression spring:1',
'Installed compression spring:1','Installed compression spring:1',#15223,
#15238,'Installed compression spring:1');
#206=NEXT_ASSEMBLY_USAGE_OCCURRENCE('Column brace:1','Column brace:1',
'Column brace:1',#15223,#15239,'Column brace:1');
#207=NEXT_ASSEMBLY_USAGE_OCCURRENCE('Column brace (1):1',
'Column brace (1):1','Column brace (1):1',#15223,#15240,
'Column brace (1):1');
#208=NEXT_ASSEMBLY_USAGE_OCCURRENCE(
'Slotted Extrusion - 20 x 20 x 400 mm:2',
'Slotted Extrusion - 20 x 20 x 400 mm:2',
'Slotted Extrusion - 20 x 20 x 400 mm:2',#15223,#15241,
'Slotted Extrusion - 20 x 20 x 400 mm:2');
#209=NEXT_ASSEMBLY_USAGE_OCCURRENCE('Cap Screw - M5x20:2',
'Cap Screw - M5x20:2','Cap Screw - M5x20:2',#15223,#15244,
'Cap Screw - M5x20:2');
#210=NEXT_ASSEMBLY_USAGE_OCCURRENCE('Cap Screw - M5x20:3',
'Cap Screw - M5x20:3','Cap Screw - M5x20:3',#15223,#15244,
'Cap Screw - M5x20:3');
#211=NEXT_ASSEMBLY_USAGE_OCCURRENCE('Captive slot nut:2',
'Captive slot nut:2','Captive slot nut:2',#15223,#15245,
'Captive slot nut:2');
#212=NEXT_ASSEMBLY_USAGE_OCCURRENCE('Flat Washer - M5:2',
'Flat Washer - M5:2','Flat Washer - M5:2',#15223,#15246,
'Flat Washer - M5:2');
#213=NEXT_ASSEMBLY_USAGE_OCCURRENCE('M5x14 Cap Screw:2',
'M5x14 Cap Screw:2','M5x14 Cap Screw:2',#15223,#15259,
'M5x14 Cap Screw:2');
#214=NEXT_ASSEMBLY_USAGE_OCCURRENCE('Captive slot nut:3',
'Captive slot nut:3','Captive slot nut:3',#15223,#15245,
'Captive slot nut:3');
#215=NEXT_ASSEMBLY_USAGE_OCCURRENCE('Flat Washer - M5:3',
'Flat Washer - M5:3','Flat Washer - M5:3',#15223,#15246,
'Flat Washer - M5:3');
#216=NEXT_ASSEMBLY_USAGE_OCCURRENCE('M5x14 Cap Screw:3',
'M5x14 Cap Screw:3','M5x14 Cap Screw:3',#15223,#15259,
'M5x14 Cap Screw:3');
#217=NEXT_ASSEMBLY_USAGE_OCCURRENCE(
'Linear Guide Rail - 15 mm, 220 mm Long:2',
'Linear Guide Rail - 15 mm, 220 mm Long:2',
'Linear Guide Rail - 15 mm, 220 mm Long:2',#15223,#15242,
'Linear Guide Rail - 15 mm, 220 mm Long:2');
#218=NEXT_ASSEMBLY_USAGE_OCCURRENCE('Cap Screw - M4x16:2',
'Cap Screw - M4x16:2','Cap Screw - M4x16:2',#15223,#15260,
'Cap Screw - M4x16:2');
#219=NEXT_ASSEMBLY_USAGE_OCCURRENCE('Cap Screw - M4x16:3',
'Cap Screw - M4x16:3','Cap Screw - M4x16:3',#15223,#15260,
'Cap Screw - M4x16:3');
#220=NEXT_ASSEMBLY_USAGE_OCCURRENCE('Cap Screw - M4x16:4',
'Cap Screw - M4x16:4','Cap Screw - M4x16:4',#15223,#15260,
'Cap Screw - M4x16:4');
#221=NEXT_ASSEMBLY_USAGE_OCCURRENCE('Cap Screw - M4x16:5',
'Cap Screw - M4x16:5','Cap Screw - M4x16:5',#15223,#15260,
'Cap Screw - M4x16:5');
#222=NEXT_ASSEMBLY_USAGE_OCCURRENCE('M5x30 frame screw:2',
'M5x30 frame screw:2','M5x30 frame screw:2',#15223,#15243,
'M5x30 frame screw:2');
#223=NEXT_ASSEMBLY_USAGE_OCCURRENCE('M5x30 frame screw:3',
'M5x30 frame screw:3','M5x30 frame screw:3',#15223,#15243,
'M5x30 frame screw:3');
#224=NEXT_ASSEMBLY_USAGE_OCCURRENCE('Cap Screw - M5x20:4',
'Cap Screw - M5x20:4','Cap Screw - M5x20:4',#15223,#15244,
'Cap Screw - M5x20:4');
#225=NEXT_ASSEMBLY_USAGE_OCCURRENCE('Captive slot nut:4',
'Captive slot nut:4','Captive slot nut:4',#15223,#15245,
'Captive slot nut:4');
#226=NEXT_ASSEMBLY_USAGE_OCCURRENCE('Flat Washer - M5:4',
'Flat Washer - M5:4','Flat Washer - M5:4',#15223,#15246,
'Flat Washer - M5:4');
#227=NEXT_ASSEMBLY_USAGE_OCCURRENCE('M5x14 Cap Screw:8',
'M5x14 Cap Screw:8','M5x14 Cap Screw:8',#15223,#15259,
'M5x14 Cap Screw:8');
#228=NEXT_ASSEMBLY_USAGE_OCCURRENCE('Cap Screw - M5x20:5',
'Cap Screw - M5x20:5','Cap Screw - M5x20:5',#15223,#15244,
'Cap Screw - M5x20:5');
#229=NEXT_ASSEMBLY_USAGE_OCCURRENCE('Captive slot nut:5',
'Captive slot nut:5','Captive slot nut:5',#15223,#15245,
'Captive slot nut:5');
#230=NEXT_ASSEMBLY_USAGE_OCCURRENCE('Flat Washer - M5:5',
'Flat Washer - M5:5','Flat Washer - M5:5',#15223,#15246,
'Flat Washer - M5:5');
#231=NEXT_ASSEMBLY_USAGE_OCCURRENCE('M5x14 Cap Screw:9',
'M5x14 Cap Screw:9','M5x14 Cap Screw:9',#15223,#15259,
'M5x14 Cap Screw:9');
#232=NEXT_ASSEMBLY_USAGE_OCCURRENCE('Platform and carriage bracket:1',
'Platform and carriage bracket:1','Platform and carriage bracket:1',#15247,
#15248,'Platform and carriage bracket:1');
#233=NEXT_ASSEMBLY_USAGE_OCCURRENCE('Spring piston:1','Spring piston:1',
'Spring piston:1',#15247,#15249,'Spring piston:1');
#234=NEXT_ASSEMBLY_USAGE_OCCURRENCE('Counterbalance rod:1',
'Counterbalance rod:1','Counterbalance rod:1',#15247,#15250,
'Counterbalance rod:1');
#235=NEXT_ASSEMBLY_USAGE_OCCURRENCE('M10 rod nut:1','M10 rod nut:1',
'M10 rod nut:1',#15247,#15251,'M10 rod nut:1');
#236=NEXT_ASSEMBLY_USAGE_OCCURRENCE('Lock bracket:1','Lock bracket:1',
'Lock bracket:1',#15247,#15252,'Lock bracket:1');
#237=NEXT_ASSEMBLY_USAGE_OCCURRENCE('Retracted lock shoe:1',
'Retracted lock shoe:1','Retracted lock shoe:1',#15247,#15253,
'Retracted lock shoe:1');
#238=NEXT_ASSEMBLY_USAGE_OCCURRENCE('Lock screw and knob:1',
'Lock screw and knob:1','Lock screw and knob:1',#15247,#15254,
'Lock screw and knob:1');
#239=NEXT_ASSEMBLY_USAGE_OCCURRENCE(
'Flanged Linear Guide Carriage - 15 mm:2',
'Flanged Linear Guide Carriage - 15 mm:2',
'Flanged Linear Guide Carriage - 15 mm:2',#15247,#15255,
'Flanged Linear Guide Carriage - 15 mm:2');
#240=NEXT_ASSEMBLY_USAGE_OCCURRENCE('M5x14 Cap Screw:4',
'M5x14 Cap Screw:4','M5x14 Cap Screw:4',#15247,#15259,
'M5x14 Cap Screw:4');
#241=NEXT_ASSEMBLY_USAGE_OCCURRENCE('M5x14 Cap Screw:5',
'M5x14 Cap Screw:5','M5x14 Cap Screw:5',#15247,#15259,
'M5x14 Cap Screw:5');
#242=NEXT_ASSEMBLY_USAGE_OCCURRENCE('M5x14 Cap Screw:6',
'M5x14 Cap Screw:6','M5x14 Cap Screw:6',#15247,#15259,
'M5x14 Cap Screw:6');
#243=NEXT_ASSEMBLY_USAGE_OCCURRENCE('M5x14 Cap Screw:7',
'M5x14 Cap Screw:7','M5x14 Cap Screw:7',#15247,#15259,
'M5x14 Cap Screw:7');
#244=NEXT_ASSEMBLY_USAGE_OCCURRENCE('Cap Screw - M4x16:6',
'Cap Screw - M4x16:6','Cap Screw - M4x16:6',#15247,#15260,
'Cap Screw - M4x16:6');
#245=NEXT_ASSEMBLY_USAGE_OCCURRENCE('Column and spring barrel:1',
'Column and spring barrel:1','Column and spring barrel:1',#15222,#15223,
'Column and spring barrel:1');
#246=NEXT_ASSEMBLY_USAGE_OCCURRENCE('Moving platform and rod:1',
'Moving platform and rod:1','Moving platform and rod:1',#15222,#15247,
'Moving platform and rod:1');
#247=CONICAL_SURFACE('',#7862,0.4,0.785398163397448);
#248=CONICAL_SURFACE('',#7866,0.41,0.785398163397448);
#249=CONICAL_SURFACE('',#7870,0.26,0.463647609000806);
#250=CONICAL_SURFACE('',#7876,0.4,0.785398163397448);
#251=CONICAL_SURFACE('',#7880,0.41,0.785398163397448);
#252=CONICAL_SURFACE('',#7884,0.26,0.463647609000806);
#253=CONICAL_SURFACE('',#7888,0.225,0.785398163397448);
#254=CONICAL_SURFACE('',#7921,0.275,0.785398163397449);
#255=CONICAL_SURFACE('',#8128,0.4,0.785398163397448);
#256=CONICAL_SURFACE('',#8132,0.41,0.785398163397448);
#257=CONICAL_SURFACE('',#8136,0.26,0.463647609000806);
#258=CONICAL_SURFACE('',#8142,0.325,0.785398163397448);
#259=CONICAL_SURFACE('',#8146,0.335,0.785398163397448);
#260=CONICAL_SURFACE('',#8150,0.21,0.463647609000806);
#261=CONICAL_SURFACE('',#8154,0.18,0.785398163397448);
#262=ORIENTED_CLOSED_SHELL('',*,#7092,.F.);
#263=ORIENTED_CLOSED_SHELL('',*,#7095,.F.);
#264=ORIENTED_CLOSED_SHELL('',*,#7108,.F.);
#265=ORIENTED_CLOSED_SHELL('',*,#7111,.F.);
#266=BREP_WITH_VOIDS('Body1',#7093,(#262));
#267=BREP_WITH_VOIDS('Body1',#7094,(#263));
#268=BREP_WITH_VOIDS('Body1',#7109,(#264));
#269=BREP_WITH_VOIDS('Body1',#7110,(#265));
#270=ELLIPSE('',#7710,0.545757787392906,0.5);
#271=ELLIPSE('',#7716,1.24744637118378,0.5);
#272=ELLIPSE('',#7717,0.300166783066098,0.275);
#273=ELLIPSE('',#7732,0.545757787392906,0.5);
#274=ELLIPSE('',#7738,1.24744637118378,0.5);
#275=ELLIPSE('',#7739,0.300166783066098,0.275);
#276=ELLIPSE('',#7910,0.299389011154384,0.2117);
#277=ELLIPSE('',#7914,0.299389011154384,0.2117);
#278=B_SPLINE_CURVE_WITH_KNOTS('',3,(#13224,#13225,#13226,#13227,#13228,
#13229,#13230,#13231,#13232,#13233,#13234,#13235,#13236,#13237,#13238,#13239,
#13240,#13241,#13242,#13243,#13244,#13245,#13246,#13247,#13248,#13249,#13250,
#13251,#13252,#13253,#13254,#13255,#13256,#13257,#13258,#13259,#13260,#13261,
#13262,#13263,#13264,#13265,#13266,#13267,#13268,#13269,#13270,#13271,#13272,
#13273,#13274,#13275,#13276,#13277,#13278,#13279,#13280,#13281,#13282,#13283,
#13284,#13285,#13286,#13287,#13288,#13289,#13290,#13291,#13292,#13293,#13294,
#13295,#13296,#13297,#13298,#13299,#13300,#13301,#13302,#13303,#13304,#13305,
#13306,#13307,#13308,#13309,#13310,#13311,#13312,#13313,#13314,#13315,#13316,
#13317,#13318,#13319,#13320,#13321,#13322,#13323,#13324,#13325,#13326,#13327,
#13328,#13329,#13330,#13331,#13332,#13333,#13334,#13335,#13336,#13337,#13338,
#13339,#13340,#13341,#13342,#13343,#13344,#13345,#13346,#13347,#13348,#13349,
#13350,#13351,#13352,#13353,#13354,#13355,#13356,#13357,#13358,#13359,#13360,
#13361,#13362,#13363,#13364,#13365,#13366,#13367,#13368,#13369,#13370,#13371,
#13372,#13373,#13374,#13375,#13376,#13377,#13378,#13379,#13380,#13381,#13382,
#13383,#13384,#13385,#13386,#13387,#13388,#13389,#13390,#13391,#13392,#13393,
#13394,#13395,#13396,#13397,#13398,#13399,#13400,#13401,#13402,#13403,#13404,
#13405,#13406,#13407,#13408,#13409,#13410,#13411,#13412,#13413,#13414,#13415,
#13416,#13417,#13418,#13419,#13420,#13421,#13422,#13423,#13424,#13425,#13426,
#13427,#13428,#13429,#13430,#13431,#13432,#13433,#13434,#13435,#13436,#13437,
#13438,#13439,#13440,#13441,#13442,#13443,#13444,#13445,#13446,#13447,#13448,
#13449,#13450,#13451,#13452,#13453,#13454,#13455,#13456,#13457,#13458,#13459,
#13460,#13461,#13462,#13463),.UNSPECIFIED.,.F.,.F.,(4,1,1,1,1,1,1,1,1,1,
1,1,1,1,1,1,1,1,1,1,1,1,1,1,1,1,1,1,1,1,1,1,1,1,1,1,1,1,1,1,1,1,1,1,1,1,
1,1,1,1,1,1,1,1,1,1,1,1,1,1,1,1,1,1,1,1,1,1,1,1,1,1,1,1,1,1,1,1,1,1,1,1,
1,1,1,1,1,1,1,1,1,1,1,1,1,1,1,1,1,1,1,1,1,1,1,1,1,1,1,1,1,1,1,1,1,1,1,1,
1,1,1,1,1,1,1,1,1,1,1,1,1,1,1,1,1,1,1,1,1,1,1,1,1,1,1,1,1,1,1,1,1,1,1,1,
1,1,1,1,1,1,1,1,1,1,1,1,1,1,1,1,1,1,1,1,1,1,1,1,1,1,1,1,1,1,1,1,1,1,1,1,
1,1,1,1,1,1,1,1,1,1,1,1,1,1,1,1,1,1,1,1,1,1,1,1,1,1,1,1,1,1,1,1,1,1,1,1,
1,1,1,1,1,1,1,1,1,1,1,4),(0.,0.00446428571428571,0.00892857142857143,0.0133928571428571,
0.0178571428571429,0.0223214285714286,0.0267857142857143,0.03125,0.0357142857142857,
0.0401785714285714,0.0446428571428571,0.0491071428571428,0.0513392857142857,
0.0535714285714286,0.0580357142857143,0.0625,0.0669642857142857,0.0714285714285714,
0.0758928571428571,0.0803571428571428,0.0848214285714286,0.0892857142857143,
0.09375,0.0982142857142857,0.102678571428571,0.107142857142857,0.111607142857143,
0.116071428571429,0.120535714285714,0.125,0.129464285714286,0.133928571428571,
0.136160714285714,0.138392857142857,0.142857142857143,0.146825396825397,
0.150793650793651,0.154761904761905,0.158730158730159,0.162698412698413,
0.166666666666667,0.170634920634921,0.174603174603175,0.17989417989418,
0.185185185185185,0.19047619047619,0.194444444444444,0.198412698412698,
0.202380952380952,0.206349206349206,0.21031746031746,0.214285714285714,
0.218253968253968,0.220238095238095,0.222222222222222,0.226190476190476,
0.23015873015873,0.234126984126984,0.238095238095238,0.241071428571429,
0.244047619047619,0.247023809523809,0.25,0.25297619047619,0.255952380952381,
0.258928571428571,0.261904761904762,0.267857142857143,0.273809523809524,
0.279761904761905,0.285714285714286,0.291666666666667,0.297619047619048,
0.303571428571429,0.30952380952381,0.31547619047619,0.321428571428571,0.327380952380952,
0.333333333333333,0.339285714285714,0.345238095238095,0.351190476190476,
0.357142857142857,0.363095238095238,0.369047619047619,0.375,0.380952380952381,
0.386904761904762,0.392857142857143,0.398809523809524,0.404761904761905,
0.407738095238095,0.410714285714286,0.413690476190476,0.416666666666667,
0.419642857142857,0.422619047619048,0.425595238095238,0.428571428571429,
0.433035714285714,0.4375,0.441964285714286,0.446428571428571,0.450892857142857,
0.455357142857143,0.459821428571429,0.464285714285714,0.46875,0.473214285714286,
0.477678571428571,0.482142857142857,0.486607142857143,0.491071428571429,
0.495535714285714,0.5,0.504464285714286,0.508928571428571,0.513392857142857,
0.517857142857143,0.522321428571428,0.526785714285714,0.53125,0.535714285714286,
0.540178571428571,0.544642857142857,0.549107142857143,0.553571428571429,
0.558035714285714,0.5625,0.566964285714286,0.571428571428571,0.575892857142857,
0.580357142857143,0.584821428571428,0.589285714285714,0.59375,0.598214285714286,
0.602678571428571,0.607142857142857,0.611607142857143,0.616071428571429,
0.620535714285714,0.625,0.627232142857143,0.629464285714286,0.633928571428571,
0.638392857142857,0.642857142857143,0.645833333333333,0.648809523809524,
0.651785714285714,0.654761904761905,0.657738095238095,0.660714285714286,
0.663690476190476,0.666666666666667,0.66765873015873,0.670634920634921,
0.674603174603175,0.678571428571428,0.683035714285714,0.6875,0.691964285714286,
0.696428571428571,0.700892857142857,0.705357142857143,0.709821428571428,
0.714285714285714,0.717261904761905,0.720238095238095,0.723214285714286,
0.726190476190476,0.729166666666667,0.732142857142857,0.735119047619047,
0.738095238095238,0.744047619047619,0.75,0.755952380952381,0.761904761904762,
0.767857142857143,0.773809523809524,0.779761904761905,0.785714285714286,
0.78968253968254,0.793650793650793,0.797619047619047,0.801587301587302,
0.805555555555555,0.809523809523809,0.8125,0.81547619047619,0.818452380952381,
0.821428571428571,0.824404761904762,0.827380952380952,0.833333333333333,
0.836309523809524,0.839285714285714,0.842261904761905,0.845238095238095,
0.848214285714286,0.851190476190476,0.854166666666667,0.857142857142857,
0.861607142857143,0.866071428571429,0.870535714285714,0.875,0.879464285714286,
0.883928571428571,0.888392857142857,0.892857142857143,0.897321428571428,
0.901785714285714,0.90625,0.910714285714286,0.915178571428571,0.919642857142857,
0.924107142857143,0.928571428571429,0.930803571428571,0.933035714285714,
0.9375,0.941964285714286,0.946428571428571,0.950892857142857,0.955357142857143,
0.959821428571429,0.964285714285714,0.96875,0.973214285714286,0.977678571428572,
0.982142857142857,0.986607142857143,0.991071428571429,0.995535714285714,
1.),.UNSPECIFIED.);
#279=B_SPLINE_SURFACE_WITH_KNOTS('',3,3,((#10821,#10822,#10823,#10824,#10825,
#10826,#10827,#10828,#10829,#10830,#10831,#10832,#10833,#10834,#10835,#10836,
#10837,#10838,#10839,#10840,#10841,#10842,#10843,#10844,#10845,#10846,#10847,
#10848,#10849,#10850,#10851,#10852,#10853,#10854,#10855,#10856,#10857,#10858,
#10859,#10860,#10861,#10862,#10863,#10864,#10865,#10866,#10867,#10868,#10869,
#10870,#10871,#10872,#10873,#10874,#10875,#10876,#10877,#10878,#10879,#10880,
#10881,#10882,#10883,#10884,#10885,#10886,#10887,#10888,#10889,#10890,#10891,
#10892,#10893,#10894,#10895,#10896,#10897,#10898,#10899,#10900,#10901,#10902,
#10903,#10904,#10905,#10906,#10907,#10908,#10909,#10910,#10911,#10912,#10913,
#10914,#10915,#10916,#10917,#10918,#10919,#10920,#10921,#10922,#10923,#10924,
#10925,#10926,#10927,#10928,#10929,#10930,#10931,#10932,#10933,#10934,#10935,
#10936,#10937,#10938,#10939,#10940,#10941,#10942,#10943,#10944,#10945,#10946,
#10947,#10948,#10949,#10950,#10951,#10952,#10953,#10954,#10955,#10956,#10957,
#10958,#10959,#10960,#10961,#10962,#10963,#10964,#10965,#10966,#10967,#10968,
#10969,#10970,#10971,#10972,#10973,#10974,#10975,#10976,#10977,#10978,#10979,
#10980,#10981,#10982,#10983,#10984,#10985,#10986,#10987,#10988,#10989,#10990,
#10991,#10992,#10993,#10994,#10995,#10996,#10997,#10998,#10999,#11000,#11001,
#11002,#11003,#11004,#11005,#11006,#11007,#11008,#11009,#11010,#11011,#11012,
#11013,#11014,#11015,#11016,#11017,#11018,#11019,#11020,#11021,#11022,#11023,
#11024,#11025,#11026,#11027,#11028,#11029,#11030,#11031,#11032,#11033,#11034,
#11035,#11036,#11037,#11038,#11039,#11040,#11041,#11042,#11043,#11044,#11045,
#11046,#11047,#11048,#11049,#11050,#11051,#11052,#11053,#11054,#11055,#11056,
#11057,#11058,#11059,#11060),(#11061,#11062,#11063,#11064,#11065,#11066,
#11067,#11068,#11069,#11070,#11071,#11072,#11073,#11074,#11075,#11076,#11077,
#11078,#11079,#11080,#11081,#11082,#11083,#11084,#11085,#11086,#11087,#11088,
#11089,#11090,#11091,#11092,#11093,#11094,#11095,#11096,#11097,#11098,#11099,
#11100,#11101,#11102,#11103,#11104,#11105,#11106,#11107,#11108,#11109,#11110,
#11111,#11112,#11113,#11114,#11115,#11116,#11117,#11118,#11119,#11120,#11121,
#11122,#11123,#11124,#11125,#11126,#11127,#11128,#11129,#11130,#11131,#11132,
#11133,#11134,#11135,#11136,#11137,#11138,#11139,#11140,#11141,#11142,#11143,
#11144,#11145,#11146,#11147,#11148,#11149,#11150,#11151,#11152,#11153,#11154,
#11155,#11156,#11157,#11158,#11159,#11160,#11161,#11162,#11163,#11164,#11165,
#11166,#11167,#11168,#11169,#11170,#11171,#11172,#11173,#11174,#11175,#11176,
#11177,#11178,#11179,#11180,#11181,#11182,#11183,#11184,#11185,#11186,#11187,
#11188,#11189,#11190,#11191,#11192,#11193,#11194,#11195,#11196,#11197,#11198,
#11199,#11200,#11201,#11202,#11203,#11204,#11205,#11206,#11207,#11208,#11209,
#11210,#11211,#11212,#11213,#11214,#11215,#11216,#11217,#11218,#11219,#11220,
#11221,#11222,#11223,#11224,#11225,#11226,#11227,#11228,#11229,#11230,#11231,
#11232,#11233,#11234,#11235,#11236,#11237,#11238,#11239,#11240,#11241,#11242,
#11243,#11244,#11245,#11246,#11247,#11248,#11249,#11250,#11251,#11252,#11253,
#11254,#11255,#11256,#11257,#11258,#11259,#11260,#11261,#11262,#11263,#11264,
#11265,#11266,#11267,#11268,#11269,#11270,#11271,#11272,#11273,#11274,#11275,
#11276,#11277,#11278,#11279,#11280,#11281,#11282,#11283,#11284,#11285,#11286,
#11287,#11288,#11289,#11290,#11291,#11292,#11293,#11294,#11295,#11296,#11297,
#11298,#11299,#11300),(#11301,#11302,#11303,#11304,#11305,#11306,#11307,
#11308,#11309,#11310,#11311,#11312,#11313,#11314,#11315,#11316,#11317,#11318,
#11319,#11320,#11321,#11322,#11323,#11324,#11325,#11326,#11327,#11328,#11329,
#11330,#11331,#11332,#11333,#11334,#11335,#11336,#11337,#11338,#11339,#11340,
#11341,#11342,#11343,#11344,#11345,#11346,#11347,#11348,#11349,#11350,#11351,
#11352,#11353,#11354,#11355,#11356,#11357,#11358,#11359,#11360,#11361,#11362,
#11363,#11364,#11365,#11366,#11367,#11368,#11369,#11370,#11371,#11372,#11373,
#11374,#11375,#11376,#11377,#11378,#11379,#11380,#11381,#11382,#11383,#11384,
#11385,#11386,#11387,#11388,#11389,#11390,#11391,#11392,#11393,#11394,#11395,
#11396,#11397,#11398,#11399,#11400,#11401,#11402,#11403,#11404,#11405,#11406,
#11407,#11408,#11409,#11410,#11411,#11412,#11413,#11414,#11415,#11416,#11417,
#11418,#11419,#11420,#11421,#11422,#11423,#11424,#11425,#11426,#11427,#11428,
#11429,#11430,#11431,#11432,#11433,#11434,#11435,#11436,#11437,#11438,#11439,
#11440,#11441,#11442,#11443,#11444,#11445,#11446,#11447,#11448,#11449,#11450,
#11451,#11452,#11453,#11454,#11455,#11456,#11457,#11458,#11459,#11460,#11461,
#11462,#11463,#11464,#11465,#11466,#11467,#11468,#11469,#11470,#11471,#11472,
#11473,#11474,#11475,#11476,#11477,#11478,#11479,#11480,#11481,#11482,#11483,
#11484,#11485,#11486,#11487,#11488,#11489,#11490,#11491,#11492,#11493,#11494,
#11495,#11496,#11497,#11498,#11499,#11500,#11501,#11502,#11503,#11504,#11505,
#11506,#11507,#11508,#11509,#11510,#11511,#11512,#11513,#11514,#11515,#11516,
#11517,#11518,#11519,#11520,#11521,#11522,#11523,#11524,#11525,#11526,#11527,
#11528,#11529,#11530,#11531,#11532,#11533,#11534,#11535,#11536,#11537,#11538,
#11539,#11540),(#11541,#11542,#11543,#11544,#11545,#11546,#11547,#11548,
#11549,#11550,#11551,#11552,#11553,#11554,#11555,#11556,#11557,#11558,#11559,
#11560,#11561,#11562,#11563,#11564,#11565,#11566,#11567,#11568,#11569,#11570,
#11571,#11572,#11573,#11574,#11575,#11576,#11577,#11578,#11579,#11580,#11581,
#11582,#11583,#11584,#11585,#11586,#11587,#11588,#11589,#11590,#11591,#11592,
#11593,#11594,#11595,#11596,#11597,#11598,#11599,#11600,#11601,#11602,#11603,
#11604,#11605,#11606,#11607,#11608,#11609,#11610,#11611,#11612,#11613,#11614,
#11615,#11616,#11617,#11618,#11619,#11620,#11621,#11622,#11623,#11624,#11625,
#11626,#11627,#11628,#11629,#11630,#11631,#11632,#11633,#11634,#11635,#11636,
#11637,#11638,#11639,#11640,#11641,#11642,#11643,#11644,#11645,#11646,#11647,
#11648,#11649,#11650,#11651,#11652,#11653,#11654,#11655,#11656,#11657,#11658,
#11659,#11660,#11661,#11662,#11663,#11664,#11665,#11666,#11667,#11668,#11669,
#11670,#11671,#11672,#11673,#11674,#11675,#11676,#11677,#11678,#11679,#11680,
#11681,#11682,#11683,#11684,#11685,#11686,#11687,#11688,#11689,#11690,#11691,
#11692,#11693,#11694,#11695,#11696,#11697,#11698,#11699,#11700,#11701,#11702,
#11703,#11704,#11705,#11706,#11707,#11708,#11709,#11710,#11711,#11712,#11713,
#11714,#11715,#11716,#11717,#11718,#11719,#11720,#11721,#11722,#11723,#11724,
#11725,#11726,#11727,#11728,#11729,#11730,#11731,#11732,#11733,#11734,#11735,
#11736,#11737,#11738,#11739,#11740,#11741,#11742,#11743,#11744,#11745,#11746,
#11747,#11748,#11749,#11750,#11751,#11752,#11753,#11754,#11755,#11756,#11757,
#11758,#11759,#11760,#11761,#11762,#11763,#11764,#11765,#11766,#11767,#11768,
#11769,#11770,#11771,#11772,#11773,#11774,#11775,#11776,#11777,#11778,#11779,
#11780),(#11781,#11782,#11783,#11784,#11785,#11786,#11787,#11788,#11789,
#11790,#11791,#11792,#11793,#11794,#11795,#11796,#11797,#11798,#11799,#11800,
#11801,#11802,#11803,#11804,#11805,#11806,#11807,#11808,#11809,#11810,#11811,
#11812,#11813,#11814,#11815,#11816,#11817,#11818,#11819,#11820,#11821,#11822,
#11823,#11824,#11825,#11826,#11827,#11828,#11829,#11830,#11831,#11832,#11833,
#11834,#11835,#11836,#11837,#11838,#11839,#11840,#11841,#11842,#11843,#11844,
#11845,#11846,#11847,#11848,#11849,#11850,#11851,#11852,#11853,#11854,#11855,
#11856,#11857,#11858,#11859,#11860,#11861,#11862,#11863,#11864,#11865,#11866,
#11867,#11868,#11869,#11870,#11871,#11872,#11873,#11874,#11875,#11876,#11877,
#11878,#11879,#11880,#11881,#11882,#11883,#11884,#11885,#11886,#11887,#11888,
#11889,#11890,#11891,#11892,#11893,#11894,#11895,#11896,#11897,#11898,#11899,
#11900,#11901,#11902,#11903,#11904,#11905,#11906,#11907,#11908,#11909,#11910,
#11911,#11912,#11913,#11914,#11915,#11916,#11917,#11918,#11919,#11920,#11921,
#11922,#11923,#11924,#11925,#11926,#11927,#11928,#11929,#11930,#11931,#11932,
#11933,#11934,#11935,#11936,#11937,#11938,#11939,#11940,#11941,#11942,#11943,
#11944,#11945,#11946,#11947,#11948,#11949,#11950,#11951,#11952,#11953,#11954,
#11955,#11956,#11957,#11958,#11959,#11960,#11961,#11962,#11963,#11964,#11965,
#11966,#11967,#11968,#11969,#11970,#11971,#11972,#11973,#11974,#11975,#11976,
#11977,#11978,#11979,#11980,#11981,#11982,#11983,#11984,#11985,#11986,#11987,
#11988,#11989,#11990,#11991,#11992,#11993,#11994,#11995,#11996,#11997,#11998,
#11999,#12000,#12001,#12002,#12003,#12004,#12005,#12006,#12007,#12008,#12009,
#12010,#12011,#12012,#12013,#12014,#12015,#12016,#12017,#12018,#12019,#12020),
(#12021,#12022,#12023,#12024,#12025,#12026,#12027,#12028,#12029,#12030,
#12031,#12032,#12033,#12034,#12035,#12036,#12037,#12038,#12039,#12040,#12041,
#12042,#12043,#12044,#12045,#12046,#12047,#12048,#12049,#12050,#12051,#12052,
#12053,#12054,#12055,#12056,#12057,#12058,#12059,#12060,#12061,#12062,#12063,
#12064,#12065,#12066,#12067,#12068,#12069,#12070,#12071,#12072,#12073,#12074,
#12075,#12076,#12077,#12078,#12079,#12080,#12081,#12082,#12083,#12084,#12085,
#12086,#12087,#12088,#12089,#12090,#12091,#12092,#12093,#12094,#12095,#12096,
#12097,#12098,#12099,#12100,#12101,#12102,#12103,#12104,#12105,#12106,#12107,
#12108,#12109,#12110,#12111,#12112,#12113,#12114,#12115,#12116,#12117,#12118,
#12119,#12120,#12121,#12122,#12123,#12124,#12125,#12126,#12127,#12128,#12129,
#12130,#12131,#12132,#12133,#12134,#12135,#12136,#12137,#12138,#12139,#12140,
#12141,#12142,#12143,#12144,#12145,#12146,#12147,#12148,#12149,#12150,#12151,
#12152,#12153,#12154,#12155,#12156,#12157,#12158,#12159,#12160,#12161,#12162,
#12163,#12164,#12165,#12166,#12167,#12168,#12169,#12170,#12171,#12172,#12173,
#12174,#12175,#12176,#12177,#12178,#12179,#12180,#12181,#12182,#12183,#12184,
#12185,#12186,#12187,#12188,#12189,#12190,#12191,#12192,#12193,#12194,#12195,
#12196,#12197,#12198,#12199,#12200,#12201,#12202,#12203,#12204,#12205,#12206,
#12207,#12208,#12209,#12210,#12211,#12212,#12213,#12214,#12215,#12216,#12217,
#12218,#12219,#12220,#12221,#12222,#12223,#12224,#12225,#12226,#12227,#12228,
#12229,#12230,#12231,#12232,#12233,#12234,#12235,#12236,#12237,#12238,#12239,
#12240,#12241,#12242,#12243,#12244,#12245,#12246,#12247,#12248,#12249,#12250,
#12251,#12252,#12253,#12254,#12255,#12256,#12257,#12258,#12259,#12260),
(#12261,#12262,#12263,#12264,#12265,#12266,#12267,#12268,#12269,#12270,
#12271,#12272,#12273,#12274,#12275,#12276,#12277,#12278,#12279,#12280,#12281,
#12282,#12283,#12284,#12285,#12286,#12287,#12288,#12289,#12290,#12291,#12292,
#12293,#12294,#12295,#12296,#12297,#12298,#12299,#12300,#12301,#12302,#12303,
#12304,#12305,#12306,#12307,#12308,#12309,#12310,#12311,#12312,#12313,#12314,
#12315,#12316,#12317,#12318,#12319,#12320,#12321,#12322,#12323,#12324,#12325,
#12326,#12327,#12328,#12329,#12330,#12331,#12332,#12333,#12334,#12335,#12336,
#12337,#12338,#12339,#12340,#12341,#12342,#12343,#12344,#12345,#12346,#12347,
#12348,#12349,#12350,#12351,#12352,#12353,#12354,#12355,#12356,#12357,#12358,
#12359,#12360,#12361,#12362,#12363,#12364,#12365,#12366,#12367,#12368,#12369,
#12370,#12371,#12372,#12373,#12374,#12375,#12376,#12377,#12378,#12379,#12380,
#12381,#12382,#12383,#12384,#12385,#12386,#12387,#12388,#12389,#12390,#12391,
#12392,#12393,#12394,#12395,#12396,#12397,#12398,#12399,#12400,#12401,#12402,
#12403,#12404,#12405,#12406,#12407,#12408,#12409,#12410,#12411,#12412,#12413,
#12414,#12415,#12416,#12417,#12418,#12419,#12420,#12421,#12422,#12423,#12424,
#12425,#12426,#12427,#12428,#12429,#12430,#12431,#12432,#12433,#12434,#12435,
#12436,#12437,#12438,#12439,#12440,#12441,#12442,#12443,#12444,#12445,#12446,
#12447,#12448,#12449,#12450,#12451,#12452,#12453,#12454,#12455,#12456,#12457,
#12458,#12459,#12460,#12461,#12462,#12463,#12464,#12465,#12466,#12467,#12468,
#12469,#12470,#12471,#12472,#12473,#12474,#12475,#12476,#12477,#12478,#12479,
#12480,#12481,#12482,#12483,#12484,#12485,#12486,#12487,#12488,#12489,#12490,
#12491,#12492,#12493,#12494,#12495,#12496,#12497,#12498,#12499,#12500),
(#12501,#12502,#12503,#12504,#12505,#12506,#12507,#12508,#12509,#12510,
#12511,#12512,#12513,#12514,#12515,#12516,#12517,#12518,#12519,#12520,#12521,
#12522,#12523,#12524,#12525,#12526,#12527,#12528,#12529,#12530,#12531,#12532,
#12533,#12534,#12535,#12536,#12537,#12538,#12539,#12540,#12541,#12542,#12543,
#12544,#12545,#12546,#12547,#12548,#12549,#12550,#12551,#12552,#12553,#12554,
#12555,#12556,#12557,#12558,#12559,#12560,#12561,#12562,#12563,#12564,#12565,
#12566,#12567,#12568,#12569,#12570,#12571,#12572,#12573,#12574,#12575,#12576,
#12577,#12578,#12579,#12580,#12581,#12582,#12583,#12584,#12585,#12586,#12587,
#12588,#12589,#12590,#12591,#12592,#12593,#12594,#12595,#12596,#12597,#12598,
#12599,#12600,#12601,#12602,#12603,#12604,#12605,#12606,#12607,#12608,#12609,
#12610,#12611,#12612,#12613,#12614,#12615,#12616,#12617,#12618,#12619,#12620,
#12621,#12622,#12623,#12624,#12625,#12626,#12627,#12628,#12629,#12630,#12631,
#12632,#12633,#12634,#12635,#12636,#12637,#12638,#12639,#12640,#12641,#12642,
#12643,#12644,#12645,#12646,#12647,#12648,#12649,#12650,#12651,#12652,#12653,
#12654,#12655,#12656,#12657,#12658,#12659,#12660,#12661,#12662,#12663,#12664,
#12665,#12666,#12667,#12668,#12669,#12670,#12671,#12672,#12673,#12674,#12675,
#12676,#12677,#12678,#12679,#12680,#12681,#12682,#12683,#12684,#12685,#12686,
#12687,#12688,#12689,#12690,#12691,#12692,#12693,#12694,#12695,#12696,#12697,
#12698,#12699,#12700,#12701,#12702,#12703,#12704,#12705,#12706,#12707,#12708,
#12709,#12710,#12711,#12712,#12713,#12714,#12715,#12716,#12717,#12718,#12719,
#12720,#12721,#12722,#12723,#12724,#12725,#12726,#12727,#12728,#12729,#12730,
#12731,#12732,#12733,#12734,#12735,#12736,#12737,#12738,#12739,#12740),
(#12741,#12742,#12743,#12744,#12745,#12746,#12747,#12748,#12749,#12750,
#12751,#12752,#12753,#12754,#12755,#12756,#12757,#12758,#12759,#12760,#12761,
#12762,#12763,#12764,#12765,#12766,#12767,#12768,#12769,#12770,#12771,#12772,
#12773,#12774,#12775,#12776,#12777,#12778,#12779,#12780,#12781,#12782,#12783,
#12784,#12785,#12786,#12787,#12788,#12789,#12790,#12791,#12792,#12793,#12794,
#12795,#12796,#12797,#12798,#12799,#12800,#12801,#12802,#12803,#12804,#12805,
#12806,#12807,#12808,#12809,#12810,#12811,#12812,#12813,#12814,#12815,#12816,
#12817,#12818,#12819,#12820,#12821,#12822,#12823,#12824,#12825,#12826,#12827,
#12828,#12829,#12830,#12831,#12832,#12833,#12834,#12835,#12836,#12837,#12838,
#12839,#12840,#12841,#12842,#12843,#12844,#12845,#12846,#12847,#12848,#12849,
#12850,#12851,#12852,#12853,#12854,#12855,#12856,#12857,#12858,#12859,#12860,
#12861,#12862,#12863,#12864,#12865,#12866,#12867,#12868,#12869,#12870,#12871,
#12872,#12873,#12874,#12875,#12876,#12877,#12878,#12879,#12880,#12881,#12882,
#12883,#12884,#12885,#12886,#12887,#12888,#12889,#12890,#12891,#12892,#12893,
#12894,#12895,#12896,#12897,#12898,#12899,#12900,#12901,#12902,#12903,#12904,
#12905,#12906,#12907,#12908,#12909,#12910,#12911,#12912,#12913,#12914,#12915,
#12916,#12917,#12918,#12919,#12920,#12921,#12922,#12923,#12924,#12925,#12926,
#12927,#12928,#12929,#12930,#12931,#12932,#12933,#12934,#12935,#12936,#12937,
#12938,#12939,#12940,#12941,#12942,#12943,#12944,#12945,#12946,#12947,#12948,
#12949,#12950,#12951,#12952,#12953,#12954,#12955,#12956,#12957,#12958,#12959,
#12960,#12961,#12962,#12963,#12964,#12965,#12966,#12967,#12968,#12969,#12970,
#12971,#12972,#12973,#12974,#12975,#12976,#12977,#12978,#12979,#12980),
(#12981,#12982,#12983,#12984,#12985,#12986,#12987,#12988,#12989,#12990,
#12991,#12992,#12993,#12994,#12995,#12996,#12997,#12998,#12999,#13000,#13001,
#13002,#13003,#13004,#13005,#13006,#13007,#13008,#13009,#13010,#13011,#13012,
#13013,#13014,#13015,#13016,#13017,#13018,#13019,#13020,#13021,#13022,#13023,
#13024,#13025,#13026,#13027,#13028,#13029,#13030,#13031,#13032,#13033,#13034,
#13035,#13036,#13037,#13038,#13039,#13040,#13041,#13042,#13043,#13044,#13045,
#13046,#13047,#13048,#13049,#13050,#13051,#13052,#13053,#13054,#13055,#13056,
#13057,#13058,#13059,#13060,#13061,#13062,#13063,#13064,#13065,#13066,#13067,
#13068,#13069,#13070,#13071,#13072,#13073,#13074,#13075,#13076,#13077,#13078,
#13079,#13080,#13081,#13082,#13083,#13084,#13085,#13086,#13087,#13088,#13089,
#13090,#13091,#13092,#13093,#13094,#13095,#13096,#13097,#13098,#13099,#13100,
#13101,#13102,#13103,#13104,#13105,#13106,#13107,#13108,#13109,#13110,#13111,
#13112,#13113,#13114,#13115,#13116,#13117,#13118,#13119,#13120,#13121,#13122,
#13123,#13124,#13125,#13126,#13127,#13128,#13129,#13130,#13131,#13132,#13133,
#13134,#13135,#13136,#13137,#13138,#13139,#13140,#13141,#13142,#13143,#13144,
#13145,#13146,#13147,#13148,#13149,#13150,#13151,#13152,#13153,#13154,#13155,
#13156,#13157,#13158,#13159,#13160,#13161,#13162,#13163,#13164,#13165,#13166,
#13167,#13168,#13169,#13170,#13171,#13172,#13173,#13174,#13175,#13176,#13177,
#13178,#13179,#13180,#13181,#13182,#13183,#13184,#13185,#13186,#13187,#13188,
#13189,#13190,#13191,#13192,#13193,#13194,#13195,#13196,#13197,#13198,#13199,
#13200,#13201,#13202,#13203,#13204,#13205,#13206,#13207,#13208,#13209,#13210,
#13211,#13212,#13213,#13214,#13215,#13216,#13217,#13218,#13219,#13220)),
 .UNSPECIFIED.,.T.,.F.,.F.,(4,1,1,1,1,1,1,4),(4,1,1,1,1,1,1,1,1,1,1,1,1,
1,1,1,1,1,1,1,1,1,1,1,1,1,1,1,1,1,1,1,1,1,1,1,1,1,1,1,1,1,1,1,1,1,1,1,1,
1,1,1,1,1,1,1,1,1,1,1,1,1,1,1,1,1,1,1,1,1,1,1,1,1,1,1,1,1,1,1,1,1,1,1,1,
1,1,1,1,1,1,1,1,1,1,1,1,1,1,1,1,1,1,1,1,1,1,1,1,1,1,1,1,1,1,1,1,1,1,1,1,
1,1,1,1,1,1,1,1,1,1,1,1,1,1,1,1,1,1,1,1,1,1,1,1,1,1,1,1,1,1,1,1,1,1,1,1,
1,1,1,1,1,1,1,1,1,1,1,1,1,1,1,1,1,1,1,1,1,1,1,1,1,1,1,1,1,1,1,1,1,1,1,1,
1,1,1,1,1,1,1,1,1,1,1,1,1,1,1,1,1,1,1,1,1,1,1,1,1,1,1,1,1,1,1,1,1,1,1,1,
1,1,1,1,1,1,1,1,4),(-3.14159265358979,-2.24399475256414,-1.34639685153848,
-0.448798950512828,0.448798950512828,1.34639685153848,2.24399475256414,
3.14159265358979),(0.,0.00446428571428571,0.00892857142857143,0.0133928571428571,
0.0178571428571429,0.0223214285714286,0.0267857142857143,0.03125,0.0357142857142857,
0.0401785714285714,0.0446428571428571,0.0491071428571428,0.0513392857142857,
0.0535714285714286,0.0580357142857143,0.0625,0.0669642857142857,0.0714285714285714,
0.0758928571428571,0.0803571428571428,0.0848214285714286,0.0892857142857143,
0.09375,0.0982142857142857,0.102678571428571,0.107142857142857,0.111607142857143,
0.116071428571429,0.120535714285714,0.125,0.129464285714286,0.133928571428571,
0.136160714285714,0.138392857142857,0.142857142857143,0.146825396825397,
0.150793650793651,0.154761904761905,0.158730158730159,0.162698412698413,
0.166666666666667,0.170634920634921,0.174603174603175,0.17989417989418,
0.185185185185185,0.19047619047619,0.194444444444444,0.198412698412698,
0.202380952380952,0.206349206349206,0.21031746031746,0.214285714285714,
0.218253968253968,0.220238095238095,0.222222222222222,0.226190476190476,
0.23015873015873,0.234126984126984,0.238095238095238,0.241071428571429,
0.244047619047619,0.247023809523809,0.25,0.25297619047619,0.255952380952381,
0.258928571428571,0.261904761904762,0.267857142857143,0.273809523809524,
0.279761904761905,0.285714285714286,0.291666666666667,0.297619047619048,
0.303571428571429,0.30952380952381,0.31547619047619,0.321428571428571,0.327380952380952,
0.333333333333333,0.339285714285714,0.345238095238095,0.351190476190476,
0.357142857142857,0.363095238095238,0.369047619047619,0.375,0.380952380952381,
0.386904761904762,0.392857142857143,0.398809523809524,0.404761904761905,
0.407738095238095,0.410714285714286,0.413690476190476,0.416666666666667,
0.419642857142857,0.422619047619048,0.425595238095238,0.428571428571429,
0.433035714285714,0.4375,0.441964285714286,0.446428571428571,0.450892857142857,
0.455357142857143,0.459821428571429,0.464285714285714,0.46875,0.473214285714286,
0.477678571428571,0.482142857142857,0.486607142857143,0.491071428571429,
0.495535714285714,0.5,0.504464285714286,0.508928571428571,0.513392857142857,
0.517857142857143,0.522321428571428,0.526785714285714,0.53125,0.535714285714286,
0.540178571428571,0.544642857142857,0.549107142857143,0.553571428571429,
0.558035714285714,0.5625,0.566964285714286,0.571428571428571,0.575892857142857,
0.580357142857143,0.584821428571428,0.589285714285714,0.59375,0.598214285714286,
0.602678571428571,0.607142857142857,0.611607142857143,0.616071428571429,
0.620535714285714,0.625,0.627232142857143,0.629464285714286,0.633928571428571,
0.638392857142857,0.642857142857143,0.645833333333333,0.648809523809524,
0.651785714285714,0.654761904761905,0.657738095238095,0.660714285714286,
0.663690476190476,0.666666666666667,0.66765873015873,0.670634920634921,
0.674603174603175,0.678571428571428,0.683035714285714,0.6875,0.691964285714286,
0.696428571428571,0.700892857142857,0.705357142857143,0.709821428571428,
0.714285714285714,0.717261904761905,0.720238095238095,0.723214285714286,
0.726190476190476,0.729166666666667,0.732142857142857,0.735119047619047,
0.738095238095238,0.744047619047619,0.75,0.755952380952381,0.761904761904762,
0.767857142857143,0.773809523809524,0.779761904761905,0.785714285714286,
0.78968253968254,0.793650793650793,0.797619047619047,0.801587301587302,
0.805555555555555,0.809523809523809,0.8125,0.81547619047619,0.818452380952381,
0.821428571428571,0.824404761904762,0.827380952380952,0.833333333333333,
0.836309523809524,0.839285714285714,0.842261904761905,0.845238095238095,
0.848214285714286,0.851190476190476,0.854166666666667,0.857142857142857,
0.861607142857143,0.866071428571429,0.870535714285714,0.875,0.879464285714286,
0.883928571428571,0.888392857142857,0.892857142857143,0.897321428571428,
0.901785714285714,0.90625,0.910714285714286,0.915178571428571,0.919642857142857,
0.924107142857143,0.928571428571429,0.930803571428571,0.933035714285714,
0.9375,0.941964285714286,0.946428571428571,0.950892857142857,0.955357142857143,
0.959821428571429,0.964285714285714,0.96875,0.973214285714286,0.977678571428572,
0.982142857142857,0.986607142857143,0.991071428571429,0.995535714285714,
1.),.UNSPECIFIED.);
#280=SHAPE_REPRESENTATION_RELATIONSHIP('SRR','None',#15184,#315);
#281=SHAPE_REPRESENTATION_RELATIONSHIP('SRR','None',#15185,#316);
#282=SHAPE_REPRESENTATION_RELATIONSHIP('SRR','None',#15186,#317);
#283=SHAPE_REPRESENTATION_RELATIONSHIP('SRR','None',#15187,#318);
#284=SHAPE_REPRESENTATION_RELATIONSHIP('SRR','None',#15188,#319);
#285=SHAPE_REPRESENTATION_RELATIONSHIP('SRR','None',#15189,#320);
#286=SHAPE_REPRESENTATION_RELATIONSHIP('SRR','None',#15190,#321);
#287=SHAPE_REPRESENTATION_RELATIONSHIP('SRR','None',#15191,#322);
#288=SHAPE_REPRESENTATION_RELATIONSHIP('SRR','None',#15192,#323);
#289=SHAPE_REPRESENTATION_RELATIONSHIP('SRR','None',#15193,#324);
#290=SHAPE_REPRESENTATION_RELATIONSHIP('SRR','None',#15194,#325);
#291=SHAPE_REPRESENTATION_RELATIONSHIP('SRR','None',#15195,#326);
#292=SHAPE_REPRESENTATION_RELATIONSHIP('SRR','None',#15196,#327);
#293=SHAPE_REPRESENTATION_RELATIONSHIP('SRR','None',#15197,#328);
#294=SHAPE_REPRESENTATION_RELATIONSHIP('SRR','None',#15198,#329);
#295=SHAPE_REPRESENTATION_RELATIONSHIP('SRR','None',#15199,#330);
#296=SHAPE_REPRESENTATION_RELATIONSHIP('SRR','None',#15200,#331);
#297=SHAPE_REPRESENTATION_RELATIONSHIP('SRR','None',#15201,#332);
#298=SHAPE_REPRESENTATION_RELATIONSHIP('SRR','None',#15202,#333);
#299=SHAPE_REPRESENTATION_RELATIONSHIP('SRR','None',#15203,#334);
#300=SHAPE_REPRESENTATION_RELATIONSHIP('SRR','None',#15204,#335);
#301=SHAPE_REPRESENTATION_RELATIONSHIP('SRR','None',#15205,#336);
#302=SHAPE_REPRESENTATION_RELATIONSHIP('SRR','None',#15206,#337);
#303=SHAPE_REPRESENTATION_RELATIONSHIP('SRR','None',#15208,#338);
#304=SHAPE_REPRESENTATION_RELATIONSHIP('SRR','None',#15209,#339);
#305=SHAPE_REPRESENTATION_RELATIONSHIP('SRR','None',#15210,#340);
#306=SHAPE_REPRESENTATION_RELATIONSHIP('SRR','None',#15211,#341);
#307=SHAPE_REPRESENTATION_RELATIONSHIP('SRR','None',#15212,#342);
#308=SHAPE_REPRESENTATION_RELATIONSHIP('SRR','None',#15213,#343);
#309=SHAPE_REPRESENTATION_RELATIONSHIP('SRR','None',#15214,#344);
#310=SHAPE_REPRESENTATION_RELATIONSHIP('SRR','None',#15216,#345);
#311=SHAPE_REPRESENTATION_RELATIONSHIP('SRR','None',#15217,#346);
#312=SHAPE_REPRESENTATION_RELATIONSHIP('SRR','None',#15218,#347);
#313=SHAPE_REPRESENTATION_RELATIONSHIP('SRR','None',#15219,#348);
#314=SHAPE_REPRESENTATION_RELATIONSHIP('SRR','None',#15220,#349);
#315=ADVANCED_BREP_SHAPE_REPRESENTATION('',(#385),#15003);
#316=ADVANCED_BREP_SHAPE_REPRESENTATION('',(#386),#15004);
#317=ADVANCED_BREP_SHAPE_REPRESENTATION('',(#387),#15005);
#318=ADVANCED_BREP_SHAPE_REPRESENTATION('',(#388),#15006);
#319=ADVANCED_BREP_SHAPE_REPRESENTATION('',(#389),#15007);
#320=ADVANCED_BREP_SHAPE_REPRESENTATION('',(#390),#15008);
#321=ADVANCED_BREP_SHAPE_REPRESENTATION('',(#391),#15009);
#322=ADVANCED_BREP_SHAPE_REPRESENTATION('',(#392),#15010);
#323=ADVANCED_BREP_SHAPE_REPRESENTATION('',(#393),#15011);
#324=ADVANCED_BREP_SHAPE_REPRESENTATION('',(#394),#15012);
#325=ADVANCED_BREP_SHAPE_REPRESENTATION('',(#395),#15013);
#326=ADVANCED_BREP_SHAPE_REPRESENTATION('',(#396),#15014);
#327=ADVANCED_BREP_SHAPE_REPRESENTATION('',(#397),#15015);
#328=ADVANCED_BREP_SHAPE_REPRESENTATION('',(#398),#15016);
#329=ADVANCED_BREP_SHAPE_REPRESENTATION('',(#399),#15017);
#330=ADVANCED_BREP_SHAPE_REPRESENTATION('',(#400),#15018);
#331=ADVANCED_BREP_SHAPE_REPRESENTATION('',(#401),#15019);
#332=ADVANCED_BREP_SHAPE_REPRESENTATION('',(#402),#15020);
#333=ADVANCED_BREP_SHAPE_REPRESENTATION('',(#403),#15021);
#334=ADVANCED_BREP_SHAPE_REPRESENTATION('',(#266),#15022);
#335=ADVANCED_BREP_SHAPE_REPRESENTATION('',(#267),#15023);
#336=ADVANCED_BREP_SHAPE_REPRESENTATION('',(#404),#15024);
#337=ADVANCED_BREP_SHAPE_REPRESENTATION('',(#405),#15025);
#338=ADVANCED_BREP_SHAPE_REPRESENTATION('',(#406),#15027);
#339=ADVANCED_BREP_SHAPE_REPRESENTATION('',(#407),#15028);
#340=ADVANCED_BREP_SHAPE_REPRESENTATION('',(#408),#15029);
#341=ADVANCED_BREP_SHAPE_REPRESENTATION('',(#409),#15030);
#342=ADVANCED_BREP_SHAPE_REPRESENTATION('',(#410),#15031);
#343=ADVANCED_BREP_SHAPE_REPRESENTATION('',(#411),#15032);
#344=ADVANCED_BREP_SHAPE_REPRESENTATION('',(#412),#15033);
#345=ADVANCED_BREP_SHAPE_REPRESENTATION('',(#413),#15035);
#346=ADVANCED_BREP_SHAPE_REPRESENTATION('',(#414),#15036);
#347=ADVANCED_BREP_SHAPE_REPRESENTATION('',(#415),#15037);
#348=ADVANCED_BREP_SHAPE_REPRESENTATION('',(#268),#15038);
#349=ADVANCED_BREP_SHAPE_REPRESENTATION('',(#269),#15039);
#350=STYLED_ITEM('',(#15436),#385);
#351=STYLED_ITEM('',(#15443),#386);
#352=STYLED_ITEM('',(#15443),#387);
#353=STYLED_ITEM('',(#15471),#388);
#354=STYLED_ITEM('',(#15443),#389);
#355=STYLED_ITEM('',(#15443),#390);
#356=STYLED_ITEM('',(#15443),#391);
#357=STYLED_ITEM('',(#15457),#392);
#358=STYLED_ITEM('',(#15457),#393);
#359=STYLED_ITEM('',(#15457),#394);
#360=STYLED_ITEM('',(#15464),#395);
#361=STYLED_ITEM('',(#15464),#396);
#362=STYLED_ITEM('',(#15464),#397);
#363=STYLED_ITEM('',(#15464),#398);
#364=STYLED_ITEM('',(#15457),#399);
#365=STYLED_ITEM('',(#15471),#400);
#366=STYLED_ITEM('',(#15471),#401);
#367=STYLED_ITEM('',(#15443),#402);
#368=STYLED_ITEM('',(#15450),#403);
#369=STYLED_ITEM('',(#15464),#266);
#370=STYLED_ITEM('',(#15464),#267);
#371=STYLED_ITEM('',(#15464),#404);
#372=STYLED_ITEM('',(#15464),#405);
#373=STYLED_ITEM('',(#15436),#406);
#374=STYLED_ITEM('',(#15457),#407);
#375=STYLED_ITEM('',(#15457),#408);
#376=STYLED_ITEM('',(#15464),#409);
#377=STYLED_ITEM('',(#15436),#410);
#378=STYLED_ITEM('',(#15450),#411);
#379=STYLED_ITEM('',(#15464),#412);
#380=STYLED_ITEM('',(#15436),#413);
#381=STYLED_ITEM('',(#15450),#414);
#382=STYLED_ITEM('',(#15471),#415);
#383=STYLED_ITEM('',(#15464),#268);
#384=STYLED_ITEM('',(#15464),#269);
#385=MANIFOLD_SOLID_BREP('Body1',#7073);
#386=MANIFOLD_SOLID_BREP('Body1',#7074);
#387=MANIFOLD_SOLID_BREP('Body1',#7075);
#388=MANIFOLD_SOLID_BREP('Body1',#7076);
#389=MANIFOLD_SOLID_BREP('Body1',#7077);
#390=MANIFOLD_SOLID_BREP('Body1',#7078);
#391=MANIFOLD_SOLID_BREP('Body1',#7079);
#392=MANIFOLD_SOLID_BREP('Body1',#7080);
#393=MANIFOLD_SOLID_BREP('Body1',#7081);
#394=MANIFOLD_SOLID_BREP('Body1',#7082);
#395=MANIFOLD_SOLID_BREP('Body1',#7083);
#396=MANIFOLD_SOLID_BREP('Body1',#7084);
#397=MANIFOLD_SOLID_BREP('Body1',#7085);
#398=MANIFOLD_SOLID_BREP('Body1',#7086);
#399=MANIFOLD_SOLID_BREP('Body1',#7087);
#400=MANIFOLD_SOLID_BREP('Body1',#7088);
#401=MANIFOLD_SOLID_BREP('Body1',#7089);
#402=MANIFOLD_SOLID_BREP('Body1',#7090);
#403=MANIFOLD_SOLID_BREP('Body1',#7091);
#404=MANIFOLD_SOLID_BREP('Body1',#7096);
#405=MANIFOLD_SOLID_BREP('Body1',#7097);
#406=MANIFOLD_SOLID_BREP('Body1',#7098);
#407=MANIFOLD_SOLID_BREP('Body1',#7099);
#408=MANIFOLD_SOLID_BREP('Body1',#7100);
#409=MANIFOLD_SOLID_BREP('Body1',#7101);
#410=MANIFOLD_SOLID_BREP('Body1',#7102);
#411=MANIFOLD_SOLID_BREP('Body1',#7103);
#412=MANIFOLD_SOLID_BREP('Body1',#7104);
#413=MANIFOLD_SOLID_BREP('Body1',#7105);
#414=MANIFOLD_SOLID_BREP('Body1',#7106);
#415=MANIFOLD_SOLID_BREP('Body1',#7107);
#416=FACE_BOUND('',#1245,.T.);
#417=FACE_BOUND('',#1246,.T.);
#418=FACE_BOUND('',#1247,.T.);
#419=FACE_BOUND('',#1248,.T.);
#420=FACE_BOUND('',#1249,.T.);
#421=FACE_BOUND('',#1251,.T.);
#422=FACE_BOUND('',#1270,.T.);
#423=FACE_BOUND('',#1272,.T.);
#424=FACE_BOUND('',#1285,.T.);
#425=FACE_BOUND('',#1286,.T.);
#426=FACE_BOUND('',#1287,.T.);
#427=FACE_BOUND('',#1288,.T.);
#428=FACE_BOUND('',#1289,.T.);
#429=FACE_BOUND('',#1290,.T.);
#430=FACE_BOUND('',#1291,.T.);
#431=FACE_BOUND('',#1292,.T.);
#432=FACE_BOUND('',#1296,.T.);
#433=FACE_BOUND('',#1297,.T.);
#434=FACE_BOUND('',#1298,.T.);
#435=FACE_BOUND('',#1299,.T.);
#436=FACE_BOUND('',#1300,.T.);
#437=FACE_BOUND('',#1301,.T.);
#438=FACE_BOUND('',#1302,.T.);
#439=FACE_BOUND('',#1303,.T.);
#440=FACE_BOUND('',#1310,.T.);
#441=FACE_BOUND('',#1313,.T.);
#442=FACE_BOUND('',#1319,.T.);
#443=FACE_BOUND('',#1322,.T.);
#444=FACE_BOUND('',#1330,.T.);
#445=FACE_BOUND('',#1332,.T.);
#446=FACE_BOUND('',#1333,.T.);
#447=FACE_BOUND('',#1334,.T.);
#448=FACE_BOUND('',#1338,.T.);
#449=FACE_BOUND('',#1339,.T.);
#450=FACE_BOUND('',#1343,.T.);
#451=FACE_BOUND('',#1345,.T.);
#452=FACE_BOUND('',#1350,.T.);
#453=FACE_BOUND('',#1353,.T.);
#454=FACE_BOUND('',#1357,.T.);
#455=FACE_BOUND('',#1358,.T.);
#456=FACE_BOUND('',#1359,.T.);
#457=FACE_BOUND('',#1361,.T.);
#458=FACE_BOUND('',#1362,.T.);
#459=FACE_BOUND('',#1363,.T.);
#460=FACE_BOUND('',#1365,.T.);
#461=FACE_BOUND('',#1367,.T.);
#462=FACE_BOUND('',#1376,.T.);
#463=FACE_BOUND('',#1378,.T.);
#464=FACE_BOUND('',#1380,.T.);
#465=FACE_BOUND('',#1382,.T.);
#466=FACE_BOUND('',#1391,.T.);
#467=FACE_BOUND('',#1393,.T.);
#468=FACE_BOUND('',#1400,.T.);
#469=FACE_BOUND('',#1401,.T.);
#470=FACE_BOUND('',#1404,.T.);
#471=FACE_BOUND('',#1408,.T.);
#472=FACE_BOUND('',#1410,.T.);
#473=FACE_BOUND('',#1416,.T.);
#474=FACE_BOUND('',#1417,.T.);
#475=FACE_BOUND('',#1420,.T.);
#476=FACE_BOUND('',#1424,.T.);
#477=FACE_BOUND('',#1426,.T.);
#478=FACE_BOUND('',#1475,.T.);
#479=FACE_BOUND('',#1477,.T.);
#480=FACE_BOUND('',#1480,.T.);
#481=FACE_BOUND('',#1483,.T.);
#482=FACE_BOUND('',#1486,.T.);
#483=FACE_BOUND('',#1489,.T.);
#484=FACE_BOUND('',#1499,.T.);
#485=FACE_BOUND('',#1500,.T.);
#486=FACE_BOUND('',#1501,.T.);
#487=FACE_BOUND('',#1502,.T.);
#488=FACE_BOUND('',#1509,.T.);
#489=FACE_BOUND('',#1510,.T.);
#490=FACE_BOUND('',#1511,.T.);
#491=FACE_BOUND('',#1512,.T.);
#492=FACE_BOUND('',#1525,.T.);
#493=FACE_BOUND('',#1533,.T.);
#494=FACE_BOUND('',#1541,.T.);
#495=FACE_BOUND('',#1557,.T.);
#496=FACE_BOUND('',#1572,.T.);
#497=FACE_BOUND('',#1575,.T.);
#498=FACE_BOUND('',#1588,.T.);
#499=FACE_BOUND('',#1589,.T.);
#500=FACE_BOUND('',#1590,.T.);
#501=FACE_BOUND('',#1591,.T.);
#502=FACE_BOUND('',#1592,.T.);
#503=FACE_BOUND('',#1595,.T.);
#504=FACE_BOUND('',#1596,.T.);
#505=FACE_BOUND('',#1597,.T.);
#506=FACE_BOUND('',#1609,.T.);
#507=FACE_BOUND('',#1610,.T.);
#508=FACE_BOUND('',#1611,.T.);
#509=FACE_BOUND('',#1614,.T.);
#510=FACE_BOUND('',#1615,.T.);
#511=FACE_BOUND('',#1616,.T.);
#512=FACE_BOUND('',#1617,.T.);
#513=FACE_BOUND('',#1618,.T.);
#514=FACE_BOUND('',#1625,.T.);
#515=FACE_BOUND('',#1627,.T.);
#516=FACE_BOUND('',#1633,.T.);
#517=FACE_BOUND('',#1636,.T.);
#518=FACE_BOUND('',#1639,.T.);
#519=FACE_BOUND('',#1643,.T.);
#520=FACE_BOUND('',#1645,.T.);
#521=FACE_BOUND('',#1650,.T.);
#522=FACE_BOUND('',#1653,.T.);
#523=FACE_BOUND('',#1655,.T.);
#524=FACE_BOUND('',#1667,.T.);
#525=FACE_BOUND('',#1684,.T.);
#526=FACE_BOUND('',#1685,.T.);
#527=FACE_BOUND('',#1686,.T.);
#528=FACE_BOUND('',#1687,.T.);
#529=FACE_BOUND('',#1730,.T.);
#530=FACE_BOUND('',#1738,.T.);
#531=PLANE('',#7504);
#532=PLANE('',#7508);
#533=PLANE('',#7512);
#534=PLANE('',#7516);
#535=PLANE('',#7520);
#536=PLANE('',#7521);
#537=PLANE('',#7522);
#538=PLANE('',#7523);
#539=PLANE('',#7524);
#540=PLANE('',#7525);
#541=PLANE('',#7527);
#542=PLANE('',#7528);
#543=PLANE('',#7529);
#544=PLANE('',#7530);
#545=PLANE('',#7531);
#546=PLANE('',#7532);
#547=PLANE('',#7534);
#548=PLANE('',#7535);
#549=PLANE('',#7536);
#550=PLANE('',#7537);
#551=PLANE('',#7538);
#552=PLANE('',#7539);
#553=PLANE('',#7544);
#554=PLANE('',#7545);
#555=PLANE('',#7546);
#556=PLANE('',#7547);
#557=PLANE('',#7548);
#558=PLANE('',#7549);
#559=PLANE('',#7575);
#560=PLANE('',#7576);
#561=PLANE('',#7577);
#562=PLANE('',#7578);
#563=PLANE('',#7579);
#564=PLANE('',#7580);
#565=PLANE('',#7581);
#566=PLANE('',#7582);
#567=PLANE('',#7583);
#568=PLANE('',#7584);
#569=PLANE('',#7589);
#570=PLANE('',#7590);
#571=PLANE('',#7591);
#572=PLANE('',#7592);
#573=PLANE('',#7593);
#574=PLANE('',#7594);
#575=PLANE('',#7599);
#576=PLANE('',#7600);
#577=PLANE('',#7601);
#578=PLANE('',#7602);
#579=PLANE('',#7603);
#580=PLANE('',#7604);
#581=PLANE('',#7618);
#582=PLANE('',#7619);
#583=PLANE('',#7623);
#584=PLANE('',#7624);
#585=PLANE('',#7632);
#586=PLANE('',#7633);
#587=PLANE('',#7644);
#588=PLANE('',#7649);
#589=PLANE('',#7655);
#590=PLANE('',#7656);
#591=PLANE('',#7658);
#592=PLANE('',#7661);
#593=PLANE('',#7669);
#594=PLANE('',#7670);
#595=PLANE('',#7678);
#596=PLANE('',#7679);
#597=PLANE('',#7681);
#598=PLANE('',#7684);
#599=PLANE('',#7692);
#600=PLANE('',#7693);
#601=PLANE('',#7701);
#602=PLANE('',#7702);
#603=PLANE('',#7706);
#604=PLANE('',#7707);
#605=PLANE('',#7712);
#606=PLANE('',#7715);
#607=PLANE('',#7720);
#608=PLANE('',#7726);
#609=PLANE('',#7727);
#610=PLANE('',#7728);
#611=PLANE('',#7729);
#612=PLANE('',#7734);
#613=PLANE('',#7737);
#614=PLANE('',#7742);
#615=PLANE('',#7748);
#616=PLANE('',#7749);
#617=PLANE('',#7750);
#618=PLANE('',#7751);
#619=PLANE('',#7753);
#620=PLANE('',#7754);
#621=PLANE('',#7755);
#622=PLANE('',#7756);
#623=PLANE('',#7757);
#624=PLANE('',#7758);
#625=PLANE('',#7759);
#626=PLANE('',#7760);
#627=PLANE('',#7761);
#628=PLANE('',#7762);
#629=PLANE('',#7763);
#630=PLANE('',#7764);
#631=PLANE('',#7765);
#632=PLANE('',#7766);
#633=PLANE('',#7767);
#634=PLANE('',#7768);
#635=PLANE('',#7769);
#636=PLANE('',#7770);
#637=PLANE('',#7771);
#638=PLANE('',#7772);
#639=PLANE('',#7773);
#640=PLANE('',#7774);
#641=PLANE('',#7775);
#642=PLANE('',#7776);
#643=PLANE('',#7777);
#644=PLANE('',#7778);
#645=PLANE('',#7779);
#646=PLANE('',#7780);
#647=PLANE('',#7781);
#648=PLANE('',#7782);
#649=PLANE('',#7783);
#650=PLANE('',#7784);
#651=PLANE('',#7785);
#652=PLANE('',#7786);
#653=PLANE('',#7787);
#654=PLANE('',#7788);
#655=PLANE('',#7792);
#656=PLANE('',#7793);
#657=PLANE('',#7794);
#658=PLANE('',#7795);
#659=PLANE('',#7796);
#660=PLANE('',#7797);
#661=PLANE('',#7798);
#662=PLANE('',#7799);
#663=PLANE('',#7800);
#664=PLANE('',#7801);
#665=PLANE('',#7806);
#666=PLANE('',#7811);
#667=PLANE('',#7816);
#668=PLANE('',#7821);
#669=PLANE('',#7831);
#670=PLANE('',#7832);
#671=PLANE('',#7833);
#672=PLANE('',#7834);
#673=PLANE('',#7835);
#674=PLANE('',#7836);
#675=PLANE('',#7837);
#676=PLANE('',#7838);
#677=PLANE('',#7839);
#678=PLANE('',#7840);
#679=PLANE('',#7841);
#680=PLANE('',#7842);
#681=PLANE('',#7843);
#682=PLANE('',#7844);
#683=PLANE('',#7846);
#684=PLANE('',#7847);
#685=PLANE('',#7848);
#686=PLANE('',#7849);
#687=PLANE('',#7850);
#688=PLANE('',#7851);
#689=PLANE('',#7852);
#690=PLANE('',#7853);
#691=PLANE('',#7854);
#692=PLANE('',#7859);
#693=PLANE('',#7860);
#694=PLANE('',#7868);
#695=PLANE('',#7874);
#696=PLANE('',#7882);
#697=PLANE('',#7890);
#698=PLANE('',#7891);
#699=PLANE('',#7892);
#700=PLANE('',#7893);
#701=PLANE('',#7894);
#702=PLANE('',#7895);
#703=PLANE('',#7896);
#704=PLANE('',#7897);
#705=PLANE('',#7898);
#706=PLANE('',#7900);
#707=PLANE('',#7901);
#708=PLANE('',#7902);
#709=PLANE('',#7904);
#710=PLANE('',#7905);
#711=PLANE('',#7906);
#712=PLANE('',#7907);
#713=PLANE('',#7908);
#714=PLANE('',#7909);
#715=PLANE('',#7916);
#716=PLANE('',#7917);
#717=PLANE('',#7918);
#718=PLANE('',#7919);
#719=PLANE('',#7926);
#720=PLANE('',#7930);
#721=PLANE('',#7936);
#722=PLANE('',#7937);
#723=PLANE('',#7938);
#724=PLANE('',#7939);
#725=PLANE('',#7940);
#726=PLANE('',#7953);
#727=PLANE('',#7954);
#728=PLANE('',#7962);
#729=PLANE('',#7967);
#730=PLANE('',#7972);
#731=PLANE('',#7973);
#732=PLANE('',#7974);
#733=PLANE('',#7975);
#734=PLANE('',#7976);
#735=PLANE('',#7977);
#736=PLANE('',#7978);
#737=PLANE('',#7979);
#738=PLANE('',#7980);
#739=PLANE('',#7981);
#740=PLANE('',#7982);
#741=PLANE('',#7990);
#742=PLANE('',#7991);
#743=PLANE('',#7996);
#744=PLANE('',#8000);
#745=PLANE('',#8001);
#746=PLANE('',#8006);
#747=PLANE('',#8009);
#748=PLANE('',#8017);
#749=PLANE('',#8018);
#750=PLANE('',#8026);
#751=PLANE('',#8027);
#752=PLANE('',#8028);
#753=PLANE('',#8029);
#754=PLANE('',#8030);
#755=PLANE('',#8031);
#756=PLANE('',#8032);
#757=PLANE('',#8034);
#758=PLANE('',#8035);
#759=PLANE('',#8036);
#760=PLANE('',#8037);
#761=PLANE('',#8038);
#762=PLANE('',#8039);
#763=PLANE('',#8044);
#764=PLANE('',#8045);
#765=PLANE('',#8049);
#766=PLANE('',#8052);
#767=PLANE('',#8058);
#768=PLANE('',#8064);
#769=PLANE('',#8070);
#770=PLANE('',#8076);
#771=PLANE('',#8077);
#772=PLANE('',#8078);
#773=PLANE('',#8079);
#774=PLANE('',#8080);
#775=PLANE('',#8081);
#776=PLANE('',#8082);
#777=PLANE('',#8083);
#778=PLANE('',#8084);
#779=PLANE('',#8085);
#780=PLANE('',#8086);
#781=PLANE('',#8087);
#782=PLANE('',#8088);
#783=PLANE('',#8089);
#784=PLANE('',#8091);
#785=PLANE('',#8092);
#786=PLANE('',#8093);
#787=PLANE('',#8094);
#788=PLANE('',#8095);
#789=PLANE('',#8096);
#790=PLANE('',#8097);
#791=PLANE('',#8098);
#792=PLANE('',#8099);
#793=PLANE('',#8100);
#794=PLANE('',#8102);
#795=PLANE('',#8103);
#796=PLANE('',#8104);
#797=PLANE('',#8105);
#798=PLANE('',#8106);
#799=PLANE('',#8107);
#800=PLANE('',#8108);
#801=PLANE('',#8109);
#802=PLANE('',#8110);
#803=PLANE('',#8111);
#804=PLANE('',#8116);
#805=PLANE('',#8117);
#806=PLANE('',#8118);
#807=PLANE('',#8119);
#808=PLANE('',#8120);
#809=PLANE('',#8121);
#810=PLANE('',#8122);
#811=PLANE('',#8123);
#812=PLANE('',#8124);
#813=PLANE('',#8126);
#814=PLANE('',#8134);
#815=PLANE('',#8140);
#816=PLANE('',#8148);
#817=PLANE('',#8156);
#818=PLANE('',#8157);
#819=PLANE('',#8158);
#820=PLANE('',#8159);
#821=PLANE('',#8160);
#822=PLANE('',#8161);
#823=PLANE('',#8162);
#824=PLANE('',#8163);
#825=PLANE('',#8164);
#826=FACE_OUTER_BOUND('',#1231,.T.);
#827=FACE_OUTER_BOUND('',#1232,.T.);
#828=FACE_OUTER_BOUND('',#1233,.T.);
#829=FACE_OUTER_BOUND('',#1234,.T.);
#830=FACE_OUTER_BOUND('',#1235,.T.);
#831=FACE_OUTER_BOUND('',#1236,.T.);
#832=FACE_OUTER_BOUND('',#1237,.T.);
#833=FACE_OUTER_BOUND('',#1238,.T.);
#834=FACE_OUTER_BOUND('',#1239,.T.);
#835=FACE_OUTER_BOUND('',#1240,.T.);
#836=FACE_OUTER_BOUND('',#1241,.T.);
#837=FACE_OUTER_BOUND('',#1242,.T.);
#838=FACE_OUTER_BOUND('',#1243,.T.);
#839=FACE_OUTER_BOUND('',#1244,.T.);
#840=FACE_OUTER_BOUND('',#1250,.T.);
#841=FACE_OUTER_BOUND('',#1252,.T.);
#842=FACE_OUTER_BOUND('',#1253,.T.);
#843=FACE_OUTER_BOUND('',#1254,.T.);
#844=FACE_OUTER_BOUND('',#1255,.T.);
#845=FACE_OUTER_BOUND('',#1256,.T.);
#846=FACE_OUTER_BOUND('',#1257,.T.);
#847=FACE_OUTER_BOUND('',#1258,.T.);
#848=FACE_OUTER_BOUND('',#1259,.T.);
#849=FACE_OUTER_BOUND('',#1260,.T.);
#850=FACE_OUTER_BOUND('',#1261,.T.);
#851=FACE_OUTER_BOUND('',#1262,.T.);
#852=FACE_OUTER_BOUND('',#1263,.T.);
#853=FACE_OUTER_BOUND('',#1264,.T.);
#854=FACE_OUTER_BOUND('',#1265,.T.);
#855=FACE_OUTER_BOUND('',#1266,.T.);
#856=FACE_OUTER_BOUND('',#1267,.T.);
#857=FACE_OUTER_BOUND('',#1268,.T.);
#858=FACE_OUTER_BOUND('',#1269,.T.);
#859=FACE_OUTER_BOUND('',#1271,.T.);
#860=FACE_OUTER_BOUND('',#1273,.T.);
#861=FACE_OUTER_BOUND('',#1274,.T.);
#862=FACE_OUTER_BOUND('',#1275,.T.);
#863=FACE_OUTER_BOUND('',#1276,.T.);
#864=FACE_OUTER_BOUND('',#1277,.T.);
#865=FACE_OUTER_BOUND('',#1278,.T.);
#866=FACE_OUTER_BOUND('',#1279,.T.);
#867=FACE_OUTER_BOUND('',#1280,.T.);
#868=FACE_OUTER_BOUND('',#1281,.T.);
#869=FACE_OUTER_BOUND('',#1282,.T.);
#870=FACE_OUTER_BOUND('',#1283,.T.);
#871=FACE_OUTER_BOUND('',#1284,.T.);
#872=FACE_OUTER_BOUND('',#1293,.T.);
#873=FACE_OUTER_BOUND('',#1294,.T.);
#874=FACE_OUTER_BOUND('',#1295,.T.);
#875=FACE_OUTER_BOUND('',#1304,.T.);
#876=FACE_OUTER_BOUND('',#1305,.T.);
#877=FACE_OUTER_BOUND('',#1306,.T.);
#878=FACE_OUTER_BOUND('',#1307,.T.);
#879=FACE_OUTER_BOUND('',#1308,.T.);
#880=FACE_OUTER_BOUND('',#1309,.T.);
#881=FACE_OUTER_BOUND('',#1311,.T.);
#882=FACE_OUTER_BOUND('',#1312,.T.);
#883=FACE_OUTER_BOUND('',#1314,.T.);
#884=FACE_OUTER_BOUND('',#1315,.T.);
#885=FACE_OUTER_BOUND('',#1316,.T.);
#886=FACE_OUTER_BOUND('',#1317,.T.);
#887=FACE_OUTER_BOUND('',#1318,.T.);
#888=FACE_OUTER_BOUND('',#1320,.T.);
#889=FACE_OUTER_BOUND('',#1321,.T.);
#890=FACE_OUTER_BOUND('',#1323,.T.);
#891=FACE_OUTER_BOUND('',#1324,.T.);
#892=FACE_OUTER_BOUND('',#1325,.T.);
#893=FACE_OUTER_BOUND('',#1326,.T.);
#894=FACE_OUTER_BOUND('',#1327,.T.);
#895=FACE_OUTER_BOUND('',#1328,.T.);
#896=FACE_OUTER_BOUND('',#1329,.T.);
#897=FACE_OUTER_BOUND('',#1331,.T.);
#898=FACE_OUTER_BOUND('',#1335,.T.);
#899=FACE_OUTER_BOUND('',#1336,.T.);
#900=FACE_OUTER_BOUND('',#1337,.T.);
#901=FACE_OUTER_BOUND('',#1340,.T.);
#902=FACE_OUTER_BOUND('',#1341,.T.);
#903=FACE_OUTER_BOUND('',#1342,.T.);
#904=FACE_OUTER_BOUND('',#1344,.T.);
#905=FACE_OUTER_BOUND('',#1346,.T.);
#906=FACE_OUTER_BOUND('',#1347,.T.);
#907=FACE_OUTER_BOUND('',#1348,.T.);
#908=FACE_OUTER_BOUND('',#1349,.T.);
#909=FACE_OUTER_BOUND('',#1351,.T.);
#910=FACE_OUTER_BOUND('',#1352,.T.);
#911=FACE_OUTER_BOUND('',#1354,.T.);
#912=FACE_OUTER_BOUND('',#1355,.T.);
#913=FACE_OUTER_BOUND('',#1356,.T.);
#914=FACE_OUTER_BOUND('',#1360,.T.);
#915=FACE_OUTER_BOUND('',#1364,.T.);
#916=FACE_OUTER_BOUND('',#1366,.T.);
#917=FACE_OUTER_BOUND('',#1368,.T.);
#918=FACE_OUTER_BOUND('',#1369,.T.);
#919=FACE_OUTER_BOUND('',#1370,.T.);
#920=FACE_OUTER_BOUND('',#1371,.T.);
#921=FACE_OUTER_BOUND('',#1372,.T.);
#922=FACE_OUTER_BOUND('',#1373,.T.);
#923=FACE_OUTER_BOUND('',#1374,.T.);
#924=FACE_OUTER_BOUND('',#1375,.T.);
#925=FACE_OUTER_BOUND('',#1377,.T.);
#926=FACE_OUTER_BOUND('',#1379,.T.);
#927=FACE_OUTER_BOUND('',#1381,.T.);
#928=FACE_OUTER_BOUND('',#1383,.T.);
#929=FACE_OUTER_BOUND('',#1384,.T.);
#930=FACE_OUTER_BOUND('',#1385,.T.);
#931=FACE_OUTER_BOUND('',#1386,.T.);
#932=FACE_OUTER_BOUND('',#1387,.T.);
#933=FACE_OUTER_BOUND('',#1388,.T.);
#934=FACE_OUTER_BOUND('',#1389,.T.);
#935=FACE_OUTER_BOUND('',#1390,.T.);
#936=FACE_OUTER_BOUND('',#1392,.T.);
#937=FACE_OUTER_BOUND('',#1394,.T.);
#938=FACE_OUTER_BOUND('',#1395,.T.);
#939=FACE_OUTER_BOUND('',#1396,.T.);
#940=FACE_OUTER_BOUND('',#1397,.T.);
#941=FACE_OUTER_BOUND('',#1398,.T.);
#942=FACE_OUTER_BOUND('',#1399,.T.);
#943=FACE_OUTER_BOUND('',#1402,.T.);
#944=FACE_OUTER_BOUND('',#1403,.T.);
#945=FACE_OUTER_BOUND('',#1405,.T.);
#946=FACE_OUTER_BOUND('',#1406,.T.);
#947=FACE_OUTER_BOUND('',#1407,.T.);
#948=FACE_OUTER_BOUND('',#1409,.T.);
#949=FACE_OUTER_BOUND('',#1411,.T.);
#950=FACE_OUTER_BOUND('',#1412,.T.);
#951=FACE_OUTER_BOUND('',#1413,.T.);
#952=FACE_OUTER_BOUND('',#1414,.T.);
#953=FACE_OUTER_BOUND('',#1415,.T.);
#954=FACE_OUTER_BOUND('',#1418,.T.);
#955=FACE_OUTER_BOUND('',#1419,.T.);
#956=FACE_OUTER_BOUND('',#1421,.T.);
#957=FACE_OUTER_BOUND('',#1422,.T.);
#958=FACE_OUTER_BOUND('',#1423,.T.);
#959=FACE_OUTER_BOUND('',#1425,.T.);
#960=FACE_OUTER_BOUND('',#1427,.T.);
#961=FACE_OUTER_BOUND('',#1428,.T.);
#962=FACE_OUTER_BOUND('',#1429,.T.);
#963=FACE_OUTER_BOUND('',#1430,.T.);
#964=FACE_OUTER_BOUND('',#1431,.T.);
#965=FACE_OUTER_BOUND('',#1432,.T.);
#966=FACE_OUTER_BOUND('',#1433,.T.);
#967=FACE_OUTER_BOUND('',#1434,.T.);
#968=FACE_OUTER_BOUND('',#1435,.T.);
#969=FACE_OUTER_BOUND('',#1436,.T.);
#970=FACE_OUTER_BOUND('',#1437,.T.);
#971=FACE_OUTER_BOUND('',#1438,.T.);
#972=FACE_OUTER_BOUND('',#1439,.T.);
#973=FACE_OUTER_BOUND('',#1440,.T.);
#974=FACE_OUTER_BOUND('',#1441,.T.);
#975=FACE_OUTER_BOUND('',#1442,.T.);
#976=FACE_OUTER_BOUND('',#1443,.T.);
#977=FACE_OUTER_BOUND('',#1444,.T.);
#978=FACE_OUTER_BOUND('',#1445,.T.);
#979=FACE_OUTER_BOUND('',#1446,.T.);
#980=FACE_OUTER_BOUND('',#1447,.T.);
#981=FACE_OUTER_BOUND('',#1448,.T.);
#982=FACE_OUTER_BOUND('',#1449,.T.);
#983=FACE_OUTER_BOUND('',#1450,.T.);
#984=FACE_OUTER_BOUND('',#1451,.T.);
#985=FACE_OUTER_BOUND('',#1452,.T.);
#986=FACE_OUTER_BOUND('',#1453,.T.);
#987=FACE_OUTER_BOUND('',#1454,.T.);
#988=FACE_OUTER_BOUND('',#1455,.T.);
#989=FACE_OUTER_BOUND('',#1456,.T.);
#990=FACE_OUTER_BOUND('',#1457,.T.);
#991=FACE_OUTER_BOUND('',#1458,.T.);
#992=FACE_OUTER_BOUND('',#1459,.T.);
#993=FACE_OUTER_BOUND('',#1460,.T.);
#994=FACE_OUTER_BOUND('',#1461,.T.);
#995=FACE_OUTER_BOUND('',#1462,.T.);
#996=FACE_OUTER_BOUND('',#1463,.T.);
#997=FACE_OUTER_BOUND('',#1464,.T.);
#998=FACE_OUTER_BOUND('',#1465,.T.);
#999=FACE_OUTER_BOUND('',#1466,.T.);
#1000=FACE_OUTER_BOUND('',#1467,.T.);
#1001=FACE_OUTER_BOUND('',#1468,.T.);
#1002=FACE_OUTER_BOUND('',#1469,.T.);
#1003=FACE_OUTER_BOUND('',#1470,.T.);
#1004=FACE_OUTER_BOUND('',#1471,.T.);
#1005=FACE_OUTER_BOUND('',#1472,.T.);
#1006=FACE_OUTER_BOUND('',#1473,.T.);
#1007=FACE_OUTER_BOUND('',#1474,.T.);
#1008=FACE_OUTER_BOUND('',#1476,.T.);
#1009=FACE_OUTER_BOUND('',#1478,.T.);
#1010=FACE_OUTER_BOUND('',#1479,.T.);
#1011=FACE_OUTER_BOUND('',#1481,.T.);
#1012=FACE_OUTER_BOUND('',#1482,.T.);
#1013=FACE_OUTER_BOUND('',#1484,.T.);
#1014=FACE_OUTER_BOUND('',#1485,.T.);
#1015=FACE_OUTER_BOUND('',#1487,.T.);
#1016=FACE_OUTER_BOUND('',#1488,.T.);
#1017=FACE_OUTER_BOUND('',#1490,.T.);
#1018=FACE_OUTER_BOUND('',#1491,.T.);
#1019=FACE_OUTER_BOUND('',#1492,.T.);
#1020=FACE_OUTER_BOUND('',#1493,.T.);
#1021=FACE_OUTER_BOUND('',#1494,.T.);
#1022=FACE_OUTER_BOUND('',#1495,.T.);
#1023=FACE_OUTER_BOUND('',#1496,.T.);
#1024=FACE_OUTER_BOUND('',#1497,.T.);
#1025=FACE_OUTER_BOUND('',#1498,.T.);
#1026=FACE_OUTER_BOUND('',#1503,.T.);
#1027=FACE_OUTER_BOUND('',#1504,.T.);
#1028=FACE_OUTER_BOUND('',#1505,.T.);
#1029=FACE_OUTER_BOUND('',#1506,.T.);
#1030=FACE_OUTER_BOUND('',#1507,.T.);
#1031=FACE_OUTER_BOUND('',#1508,.T.);
#1032=FACE_OUTER_BOUND('',#1513,.T.);
#1033=FACE_OUTER_BOUND('',#1514,.T.);
#1034=FACE_OUTER_BOUND('',#1515,.T.);
#1035=FACE_OUTER_BOUND('',#1516,.T.);
#1036=FACE_OUTER_BOUND('',#1517,.T.);
#1037=FACE_OUTER_BOUND('',#1518,.T.);
#1038=FACE_OUTER_BOUND('',#1519,.T.);
#1039=FACE_OUTER_BOUND('',#1520,.T.);
#1040=FACE_OUTER_BOUND('',#1521,.T.);
#1041=FACE_OUTER_BOUND('',#1522,.T.);
#1042=FACE_OUTER_BOUND('',#1523,.T.);
#1043=FACE_OUTER_BOUND('',#1524,.T.);
#1044=FACE_OUTER_BOUND('',#1526,.T.);
#1045=FACE_OUTER_BOUND('',#1527,.T.);
#1046=FACE_OUTER_BOUND('',#1528,.T.);
#1047=FACE_OUTER_BOUND('',#1529,.T.);
#1048=FACE_OUTER_BOUND('',#1530,.T.);
#1049=FACE_OUTER_BOUND('',#1531,.T.);
#1050=FACE_OUTER_BOUND('',#1532,.T.);
#1051=FACE_OUTER_BOUND('',#1534,.T.);
#1052=FACE_OUTER_BOUND('',#1535,.T.);
#1053=FACE_OUTER_BOUND('',#1536,.T.);
#1054=FACE_OUTER_BOUND('',#1537,.T.);
#1055=FACE_OUTER_BOUND('',#1538,.T.);
#1056=FACE_OUTER_BOUND('',#1539,.T.);
#1057=FACE_OUTER_BOUND('',#1540,.T.);
#1058=FACE_OUTER_BOUND('',#1542,.T.);
#1059=FACE_OUTER_BOUND('',#1543,.T.);
#1060=FACE_OUTER_BOUND('',#1544,.T.);
#1061=FACE_OUTER_BOUND('',#1545,.T.);
#1062=FACE_OUTER_BOUND('',#1546,.T.);
#1063=FACE_OUTER_BOUND('',#1547,.T.);
#1064=FACE_OUTER_BOUND('',#1548,.T.);
#1065=FACE_OUTER_BOUND('',#1549,.T.);
#1066=FACE_OUTER_BOUND('',#1550,.T.);
#1067=FACE_OUTER_BOUND('',#1551,.T.);
#1068=FACE_OUTER_BOUND('',#1552,.T.);
#1069=FACE_OUTER_BOUND('',#1553,.T.);
#1070=FACE_OUTER_BOUND('',#1554,.T.);
#1071=FACE_OUTER_BOUND('',#1555,.T.);
#1072=FACE_OUTER_BOUND('',#1556,.T.);
#1073=FACE_OUTER_BOUND('',#1558,.T.);
#1074=FACE_OUTER_BOUND('',#1559,.T.);
#1075=FACE_OUTER_BOUND('',#1560,.T.);
#1076=FACE_OUTER_BOUND('',#1561,.T.);
#1077=FACE_OUTER_BOUND('',#1562,.T.);
#1078=FACE_OUTER_BOUND('',#1563,.T.);
#1079=FACE_OUTER_BOUND('',#1564,.T.);
#1080=FACE_OUTER_BOUND('',#1565,.T.);
#1081=FACE_OUTER_BOUND('',#1566,.T.);
#1082=FACE_OUTER_BOUND('',#1567,.T.);
#1083=FACE_OUTER_BOUND('',#1568,.T.);
#1084=FACE_OUTER_BOUND('',#1569,.T.);
#1085=FACE_OUTER_BOUND('',#1570,.T.);
#1086=FACE_OUTER_BOUND('',#1571,.T.);
#1087=FACE_OUTER_BOUND('',#1573,.T.);
#1088=FACE_OUTER_BOUND('',#1574,.T.);
#1089=FACE_OUTER_BOUND('',#1576,.T.);
#1090=FACE_OUTER_BOUND('',#1577,.T.);
#1091=FACE_OUTER_BOUND('',#1578,.T.);
#1092=FACE_OUTER_BOUND('',#1579,.T.);
#1093=FACE_OUTER_BOUND('',#1580,.T.);
#1094=FACE_OUTER_BOUND('',#1581,.T.);
#1095=FACE_OUTER_BOUND('',#1582,.T.);
#1096=FACE_OUTER_BOUND('',#1583,.T.);
#1097=FACE_OUTER_BOUND('',#1584,.T.);
#1098=FACE_OUTER_BOUND('',#1585,.T.);
#1099=FACE_OUTER_BOUND('',#1586,.T.);
#1100=FACE_OUTER_BOUND('',#1587,.T.);
#1101=FACE_OUTER_BOUND('',#1593,.T.);
#1102=FACE_OUTER_BOUND('',#1594,.T.);
#1103=FACE_OUTER_BOUND('',#1598,.T.);
#1104=FACE_OUTER_BOUND('',#1599,.T.);
#1105=FACE_OUTER_BOUND('',#1600,.T.);
#1106=FACE_OUTER_BOUND('',#1601,.T.);
#1107=FACE_OUTER_BOUND('',#1602,.T.);
#1108=FACE_OUTER_BOUND('',#1603,.T.);
#1109=FACE_OUTER_BOUND('',#1604,.T.);
#1110=FACE_OUTER_BOUND('',#1605,.T.);
#1111=FACE_OUTER_BOUND('',#1606,.T.);
#1112=FACE_OUTER_BOUND('',#1607,.T.);
#1113=FACE_OUTER_BOUND('',#1608,.T.);
#1114=FACE_OUTER_BOUND('',#1612,.T.);
#1115=FACE_OUTER_BOUND('',#1613,.T.);
#1116=FACE_OUTER_BOUND('',#1619,.T.);
#1117=FACE_OUTER_BOUND('',#1620,.T.);
#1118=FACE_OUTER_BOUND('',#1621,.T.);
#1119=FACE_OUTER_BOUND('',#1622,.T.);
#1120=FACE_OUTER_BOUND('',#1623,.T.);
#1121=FACE_OUTER_BOUND('',#1624,.T.);
#1122=FACE_OUTER_BOUND('',#1626,.T.);
#1123=FACE_OUTER_BOUND('',#1628,.T.);
#1124=FACE_OUTER_BOUND('',#1629,.T.);
#1125=FACE_OUTER_BOUND('',#1630,.T.);
#1126=FACE_OUTER_BOUND('',#1631,.T.);
#1127=FACE_OUTER_BOUND('',#1632,.T.);
#1128=FACE_OUTER_BOUND('',#1634,.T.);
#1129=FACE_OUTER_BOUND('',#1635,.T.);
#1130=FACE_OUTER_BOUND('',#1637,.T.);
#1131=FACE_OUTER_BOUND('',#1638,.T.);
#1132=FACE_OUTER_BOUND('',#1640,.T.);
#1133=FACE_OUTER_BOUND('',#1641,.T.);
#1134=FACE_OUTER_BOUND('',#1642,.T.);
#1135=FACE_OUTER_BOUND('',#1644,.T.);
#1136=FACE_OUTER_BOUND('',#1646,.T.);
#1137=FACE_OUTER_BOUND('',#1647,.T.);
#1138=FACE_OUTER_BOUND('',#1648,.T.);
#1139=FACE_OUTER_BOUND('',#1649,.T.);
#1140=FACE_OUTER_BOUND('',#1651,.T.);
#1141=FACE_OUTER_BOUND('',#1652,.T.);
#1142=FACE_OUTER_BOUND('',#1654,.T.);
#1143=FACE_OUTER_BOUND('',#1656,.T.);
#1144=FACE_OUTER_BOUND('',#1657,.T.);
#1145=FACE_OUTER_BOUND('',#1658,.T.);
#1146=FACE_OUTER_BOUND('',#1659,.T.);
#1147=FACE_OUTER_BOUND('',#1660,.T.);
#1148=FACE_OUTER_BOUND('',#1661,.T.);
#1149=FACE_OUTER_BOUND('',#1662,.T.);
#1150=FACE_OUTER_BOUND('',#1663,.T.);
#1151=FACE_OUTER_BOUND('',#1664,.T.);
#1152=FACE_OUTER_BOUND('',#1665,.T.);
#1153=FACE_OUTER_BOUND('',#1666,.T.);
#1154=FACE_OUTER_BOUND('',#1668,.T.);
#1155=FACE_OUTER_BOUND('',#1669,.T.);
#1156=FACE_OUTER_BOUND('',#1670,.T.);
#1157=FACE_OUTER_BOUND('',#1671,.T.);
#1158=FACE_OUTER_BOUND('',#1672,.T.);
#1159=FACE_OUTER_BOUND('',#1673,.T.);
#1160=FACE_OUTER_BOUND('',#1674,.T.);
#1161=FACE_OUTER_BOUND('',#1675,.T.);
#1162=FACE_OUTER_BOUND('',#1676,.T.);
#1163=FACE_OUTER_BOUND('',#1677,.T.);
#1164=FACE_OUTER_BOUND('',#1678,.T.);
#1165=FACE_OUTER_BOUND('',#1679,.T.);
#1166=FACE_OUTER_BOUND('',#1680,.T.);
#1167=FACE_OUTER_BOUND('',#1681,.T.);
#1168=FACE_OUTER_BOUND('',#1682,.T.);
#1169=FACE_OUTER_BOUND('',#1683,.T.);
#1170=FACE_OUTER_BOUND('',#1688,.T.);
#1171=FACE_OUTER_BOUND('',#1689,.T.);
#1172=FACE_OUTER_BOUND('',#1690,.T.);
#1173=FACE_OUTER_BOUND('',#1691,.T.);
#1174=FACE_OUTER_BOUND('',#1692,.T.);
#1175=FACE_OUTER_BOUND('',#1693,.T.);
#1176=FACE_OUTER_BOUND('',#1694,.T.);
#1177=FACE_OUTER_BOUND('',#1695,.T.);
#1178=FACE_OUTER_BOUND('',#1696,.T.);
#1179=FACE_OUTER_BOUND('',#1697,.T.);
#1180=FACE_OUTER_BOUND('',#1698,.T.);
#1181=FACE_OUTER_BOUND('',#1699,.T.);
#1182=FACE_OUTER_BOUND('',#1700,.T.);
#1183=FACE_OUTER_BOUND('',#1701,.T.);
#1184=FACE_OUTER_BOUND('',#1702,.T.);
#1185=FACE_OUTER_BOUND('',#1703,.T.);
#1186=FACE_OUTER_BOUND('',#1704,.T.);
#1187=FACE_OUTER_BOUND('',#1705,.T.);
#1188=FACE_OUTER_BOUND('',#1706,.T.);
#1189=FACE_OUTER_BOUND('',#1707,.T.);
#1190=FACE_OUTER_BOUND('',#1708,.T.);
#1191=FACE_OUTER_BOUND('',#1709,.T.);
#1192=FACE_OUTER_BOUND('',#1710,.T.);
#1193=FACE_OUTER_BOUND('',#1711,.T.);
#1194=FACE_OUTER_BOUND('',#1712,.T.);
#1195=FACE_OUTER_BOUND('',#1713,.T.);
#1196=FACE_OUTER_BOUND('',#1714,.T.);
#1197=FACE_OUTER_BOUND('',#1715,.T.);
#1198=FACE_OUTER_BOUND('',#1716,.T.);
#1199=FACE_OUTER_BOUND('',#1717,.T.);
#1200=FACE_OUTER_BOUND('',#1718,.T.);
#1201=FACE_OUTER_BOUND('',#1719,.T.);
#1202=FACE_OUTER_BOUND('',#1720,.T.);
#1203=FACE_OUTER_BOUND('',#1721,.T.);
#1204=FACE_OUTER_BOUND('',#1722,.T.);
#1205=FACE_OUTER_BOUND('',#1723,.T.);
#1206=FACE_OUTER_BOUND('',#1724,.T.);
#1207=FACE_OUTER_BOUND('',#1725,.T.);
#1208=FACE_OUTER_BOUND('',#1726,.T.);
#1209=FACE_OUTER_BOUND('',#1727,.T.);
#1210=FACE_OUTER_BOUND('',#1728,.T.);
#1211=FACE_OUTER_BOUND('',#1729,.T.);
#1212=FACE_OUTER_BOUND('',#1731,.T.);
#1213=FACE_OUTER_BOUND('',#1732,.T.);
#1214=FACE_OUTER_BOUND('',#1733,.T.);
#1215=FACE_OUTER_BOUND('',#1734,.T.);
#1216=FACE_OUTER_BOUND('',#1735,.T.);
#1217=FACE_OUTER_BOUND('',#1736,.T.);
#1218=FACE_OUTER_BOUND('',#1737,.T.);
#1219=FACE_OUTER_BOUND('',#1739,.T.);
#1220=FACE_OUTER_BOUND('',#1740,.T.);
#1221=FACE_OUTER_BOUND('',#1741,.T.);
#1222=FACE_OUTER_BOUND('',#1742,.T.);
#1223=FACE_OUTER_BOUND('',#1743,.T.);
#1224=FACE_OUTER_BOUND('',#1744,.T.);
#1225=FACE_OUTER_BOUND('',#1745,.T.);
#1226=FACE_OUTER_BOUND('',#1746,.T.);
#1227=FACE_OUTER_BOUND('',#1747,.T.);
#1228=FACE_OUTER_BOUND('',#1748,.T.);
#1229=FACE_OUTER_BOUND('',#1749,.T.);
#1230=FACE_OUTER_BOUND('',#1750,.T.);
#1231=EDGE_LOOP('',(#4788,#4789,#4790,#4791));
#1232=EDGE_LOOP('',(#4792));
#1233=EDGE_LOOP('',(#4793,#4794,#4795,#4796));
#1234=EDGE_LOOP('',(#4797));
#1235=EDGE_LOOP('',(#4798,#4799,#4800,#4801));
#1236=EDGE_LOOP('',(#4802));
#1237=EDGE_LOOP('',(#4803,#4804,#4805,#4806));
#1238=EDGE_LOOP('',(#4807));
#1239=EDGE_LOOP('',(#4808,#4809,#4810,#4811));
#1240=EDGE_LOOP('',(#4812,#4813,#4814,#4815));
#1241=EDGE_LOOP('',(#4816,#4817,#4818,#4819));
#1242=EDGE_LOOP('',(#4820,#4821,#4822,#4823));
#1243=EDGE_LOOP('',(#4824,#4825,#4826,#4827));
#1244=EDGE_LOOP('',(#4828,#4829,#4830,#4831));
#1245=EDGE_LOOP('',(#4832));
#1246=EDGE_LOOP('',(#4833));
#1247=EDGE_LOOP('',(#4834));
#1248=EDGE_LOOP('',(#4835));
#1249=EDGE_LOOP('',(#4836));
#1250=EDGE_LOOP('',(#4837,#4838,#4839,#4840));
#1251=EDGE_LOOP('',(#4841));
#1252=EDGE_LOOP('',(#4842,#4843,#4844,#4845));
#1253=EDGE_LOOP('',(#4846,#4847,#4848,#4849));
#1254=EDGE_LOOP('',(#4850,#4851,#4852,#4853));
#1255=EDGE_LOOP('',(#4854,#4855,#4856,#4857));
#1256=EDGE_LOOP('',(#4858,#4859,#4860,#4861));
#1257=EDGE_LOOP('',(#4862,#4863,#4864,#4865));
#1258=EDGE_LOOP('',(#4866,#4867,#4868,#4869));
#1259=EDGE_LOOP('',(#4870,#4871,#4872,#4873));
#1260=EDGE_LOOP('',(#4874,#4875,#4876,#4877));
#1261=EDGE_LOOP('',(#4878,#4879,#4880,#4881));
#1262=EDGE_LOOP('',(#4882,#4883,#4884,#4885));
#1263=EDGE_LOOP('',(#4886,#4887,#4888,#4889));
#1264=EDGE_LOOP('',(#4890,#4891,#4892,#4893));
#1265=EDGE_LOOP('',(#4894,#4895,#4896,#4897));
#1266=EDGE_LOOP('',(#4898,#4899,#4900,#4901));
#1267=EDGE_LOOP('',(#4902,#4903,#4904,#4905));
#1268=EDGE_LOOP('',(#4906,#4907,#4908,#4909));
#1269=EDGE_LOOP('',(#4910,#4911,#4912,#4913));
#1270=EDGE_LOOP('',(#4914));
#1271=EDGE_LOOP('',(#4915,#4916,#4917,#4918));
#1272=EDGE_LOOP('',(#4919));
#1273=EDGE_LOOP('',(#4920,#4921,#4922,#4923));
#1274=EDGE_LOOP('',(#4924,#4925,#4926,#4927));
#1275=EDGE_LOOP('',(#4928,#4929,#4930,#4931));
#1276=EDGE_LOOP('',(#4932,#4933,#4934,#4935));
#1277=EDGE_LOOP('',(#4936,#4937,#4938,#4939));
#1278=EDGE_LOOP('',(#4940,#4941,#4942,#4943));
#1279=EDGE_LOOP('',(#4944,#4945,#4946,#4947));
#1280=EDGE_LOOP('',(#4948,#4949,#4950,#4951));
#1281=EDGE_LOOP('',(#4952,#4953,#4954,#4955));
#1282=EDGE_LOOP('',(#4956,#4957,#4958,#4959));
#1283=EDGE_LOOP('',(#4960,#4961,#4962,#4963));
#1284=EDGE_LOOP('',(#4964,#4965,#4966,#4967,#4968,#4969,#4970,#4971));
#1285=EDGE_LOOP('',(#4972));
#1286=EDGE_LOOP('',(#4973));
#1287=EDGE_LOOP('',(#4974));
#1288=EDGE_LOOP('',(#4975));
#1289=EDGE_LOOP('',(#4976));
#1290=EDGE_LOOP('',(#4977));
#1291=EDGE_LOOP('',(#4978));
#1292=EDGE_LOOP('',(#4979));
#1293=EDGE_LOOP('',(#4980,#4981,#4982,#4983));
#1294=EDGE_LOOP('',(#4984,#4985,#4986,#4987));
#1295=EDGE_LOOP('',(#4988,#4989,#4990,#4991,#4992,#4993,#4994,#4995));
#1296=EDGE_LOOP('',(#4996));
#1297=EDGE_LOOP('',(#4997));
#1298=EDGE_LOOP('',(#4998));
#1299=EDGE_LOOP('',(#4999));
#1300=EDGE_LOOP('',(#5000));
#1301=EDGE_LOOP('',(#5001));
#1302=EDGE_LOOP('',(#5002));
#1303=EDGE_LOOP('',(#5003));
#1304=EDGE_LOOP('',(#5004,#5005,#5006,#5007));
#1305=EDGE_LOOP('',(#5008,#5009,#5010,#5011));
#1306=EDGE_LOOP('',(#5012,#5013,#5014,#5015));
#1307=EDGE_LOOP('',(#5016,#5017,#5018,#5019));
#1308=EDGE_LOOP('',(#5020,#5021,#5022,#5023));
#1309=EDGE_LOOP('',(#5024,#5025,#5026,#5027));
#1310=EDGE_LOOP('',(#5028));
#1311=EDGE_LOOP('',(#5029,#5030,#5031,#5032));
#1312=EDGE_LOOP('',(#5033,#5034,#5035,#5036));
#1313=EDGE_LOOP('',(#5037));
#1314=EDGE_LOOP('',(#5038,#5039,#5040,#5041));
#1315=EDGE_LOOP('',(#5042,#5043,#5044,#5045));
#1316=EDGE_LOOP('',(#5046,#5047,#5048,#5049));
#1317=EDGE_LOOP('',(#5050,#5051,#5052,#5053));
#1318=EDGE_LOOP('',(#5054,#5055,#5056,#5057));
#1319=EDGE_LOOP('',(#5058));
#1320=EDGE_LOOP('',(#5059,#5060,#5061,#5062));
#1321=EDGE_LOOP('',(#5063,#5064,#5065,#5066));
#1322=EDGE_LOOP('',(#5067));
#1323=EDGE_LOOP('',(#5068,#5069,#5070,#5071));
#1324=EDGE_LOOP('',(#5072,#5073,#5074,#5075));
#1325=EDGE_LOOP('',(#5076,#5077,#5078,#5079));
#1326=EDGE_LOOP('',(#5080,#5081,#5082,#5083));
#1327=EDGE_LOOP('',(#5084,#5085,#5086,#5087));
#1328=EDGE_LOOP('',(#5088,#5089,#5090,#5091));
#1329=EDGE_LOOP('',(#5092));
#1330=EDGE_LOOP('',(#5093));
#1331=EDGE_LOOP('',(#5094));
#1332=EDGE_LOOP('',(#5095));
#1333=EDGE_LOOP('',(#5096));
#1334=EDGE_LOOP('',(#5097));
#1335=EDGE_LOOP('',(#5098,#5099,#5100,#5101));
#1336=EDGE_LOOP('',(#5102));
#1337=EDGE_LOOP('',(#5103));
#1338=EDGE_LOOP('',(#5104));
#1339=EDGE_LOOP('',(#5105));
#1340=EDGE_LOOP('',(#5106,#5107,#5108,#5109));
#1341=EDGE_LOOP('',(#5110,#5111,#5112,#5113));
#1342=EDGE_LOOP('',(#5114));
#1343=EDGE_LOOP('',(#5115));
#1344=EDGE_LOOP('',(#5116));
#1345=EDGE_LOOP('',(#5117));
#1346=EDGE_LOOP('',(#5118,#5119,#5120,#5121));
#1347=EDGE_LOOP('',(#5122,#5123,#5124,#5125));
#1348=EDGE_LOOP('',(#5126,#5127,#5128,#5129));
#1349=EDGE_LOOP('',(#5130));
#1350=EDGE_LOOP('',(#5131));
#1351=EDGE_LOOP('',(#5132,#5133,#5134,#5135));
#1352=EDGE_LOOP('',(#5136));
#1353=EDGE_LOOP('',(#5137));
#1354=EDGE_LOOP('',(#5138,#5139,#5140,#5141));
#1355=EDGE_LOOP('',(#5142,#5143,#5144,#5145));
#1356=EDGE_LOOP('',(#5146));
#1357=EDGE_LOOP('',(#5147));
#1358=EDGE_LOOP('',(#5148));
#1359=EDGE_LOOP('',(#5149));
#1360=EDGE_LOOP('',(#5150));
#1361=EDGE_LOOP('',(#5151));
#1362=EDGE_LOOP('',(#5152));
#1363=EDGE_LOOP('',(#5153));
#1364=EDGE_LOOP('',(#5154));
#1365=EDGE_LOOP('',(#5155));
#1366=EDGE_LOOP('',(#5156));
#1367=EDGE_LOOP('',(#5157));
#1368=EDGE_LOOP('',(#5158,#5159,#5160,#5161));
#1369=EDGE_LOOP('',(#5162,#5163,#5164,#5165));
#1370=EDGE_LOOP('',(#5166,#5167,#5168,#5169));
#1371=EDGE_LOOP('',(#5170));
#1372=EDGE_LOOP('',(#5171));
#1373=EDGE_LOOP('',(#5172,#5173,#5174,#5175));
#1374=EDGE_LOOP('',(#5176,#5177,#5178,#5179));
#1375=EDGE_LOOP('',(#5180));
#1376=EDGE_LOOP('',(#5181));
#1377=EDGE_LOOP('',(#5182));
#1378=EDGE_LOOP('',(#5183));
#1379=EDGE_LOOP('',(#5184));
#1380=EDGE_LOOP('',(#5185));
#1381=EDGE_LOOP('',(#5186));
#1382=EDGE_LOOP('',(#5187));
#1383=EDGE_LOOP('',(#5188,#5189,#5190,#5191));
#1384=EDGE_LOOP('',(#5192,#5193,#5194,#5195));
#1385=EDGE_LOOP('',(#5196,#5197,#5198,#5199));
#1386=EDGE_LOOP('',(#5200));
#1387=EDGE_LOOP('',(#5201));
#1388=EDGE_LOOP('',(#5202,#5203,#5204,#5205));
#1389=EDGE_LOOP('',(#5206,#5207,#5208,#5209));
#1390=EDGE_LOOP('',(#5210));
#1391=EDGE_LOOP('',(#5211));
#1392=EDGE_LOOP('',(#5212));
#1393=EDGE_LOOP('',(#5213));
#1394=EDGE_LOOP('',(#5214,#5215,#5216,#5217));
#1395=EDGE_LOOP('',(#5218));
#1396=EDGE_LOOP('',(#5219));
#1397=EDGE_LOOP('',(#5220,#5221));
#1398=EDGE_LOOP('',(#5222,#5223,#5224,#5225,#5226));
#1399=EDGE_LOOP('',(#5227,#5228,#5229,#5230));
#1400=EDGE_LOOP('',(#5231,#5232));
#1401=EDGE_LOOP('',(#5233,#5234,#5235,#5236));
#1402=EDGE_LOOP('',(#5237,#5238,#5239,#5240,#5241,#5242));
#1403=EDGE_LOOP('',(#5243,#5244));
#1404=EDGE_LOOP('',(#5245));
#1405=EDGE_LOOP('',(#5246,#5247));
#1406=EDGE_LOOP('',(#5248,#5249,#5250,#5251));
#1407=EDGE_LOOP('',(#5252,#5253,#5254,#5255));
#1408=EDGE_LOOP('',(#5256));
#1409=EDGE_LOOP('',(#5257,#5258,#5259,#5260));
#1410=EDGE_LOOP('',(#5261));
#1411=EDGE_LOOP('',(#5262,#5263,#5264));
#1412=EDGE_LOOP('',(#5265,#5266,#5267));
#1413=EDGE_LOOP('',(#5268,#5269));
#1414=EDGE_LOOP('',(#5270,#5271,#5272,#5273,#5274));
#1415=EDGE_LOOP('',(#5275,#5276,#5277,#5278));
#1416=EDGE_LOOP('',(#5279,#5280));
#1417=EDGE_LOOP('',(#5281,#5282,#5283,#5284));
#1418=EDGE_LOOP('',(#5285,#5286,#5287,#5288,#5289,#5290));
#1419=EDGE_LOOP('',(#5291,#5292));
#1420=EDGE_LOOP('',(#5293));
#1421=EDGE_LOOP('',(#5294,#5295));
#1422=EDGE_LOOP('',(#5296,#5297,#5298,#5299));
#1423=EDGE_LOOP('',(#5300,#5301,#5302,#5303));
#1424=EDGE_LOOP('',(#5304));
#1425=EDGE_LOOP('',(#5305,#5306,#5307,#5308));
#1426=EDGE_LOOP('',(#5309));
#1427=EDGE_LOOP('',(#5310,#5311,#5312));
#1428=EDGE_LOOP('',(#5313,#5314,#5315));
#1429=EDGE_LOOP('',(#5316,#5317,#5318,#5319));
#1430=EDGE_LOOP('',(#5320,#5321,#5322,#5323));
#1431=EDGE_LOOP('',(#5324,#5325,#5326,#5327));
#1432=EDGE_LOOP('',(#5328,#5329,#5330,#5331));
#1433=EDGE_LOOP('',(#5332,#5333,#5334,#5335));
#1434=EDGE_LOOP('',(#5336,#5337,#5338,#5339));
#1435=EDGE_LOOP('',(#5340,#5341,#5342,#5343));
#1436=EDGE_LOOP('',(#5344,#5345,#5346,#5347));
#1437=EDGE_LOOP('',(#5348,#5349,#5350,#5351));
#1438=EDGE_LOOP('',(#5352,#5353,#5354,#5355));
#1439=EDGE_LOOP('',(#5356,#5357,#5358,#5359));
#1440=EDGE_LOOP('',(#5360,#5361,#5362,#5363));
#1441=EDGE_LOOP('',(#5364,#5365,#5366,#5367));
#1442=EDGE_LOOP('',(#5368,#5369,#5370,#5371));
#1443=EDGE_LOOP('',(#5372,#5373,#5374,#5375));
#1444=EDGE_LOOP('',(#5376,#5377,#5378,#5379));
#1445=EDGE_LOOP('',(#5380,#5381,#5382,#5383));
#1446=EDGE_LOOP('',(#5384,#5385,#5386,#5387));
#1447=EDGE_LOOP('',(#5388,#5389,#5390,#5391));
#1448=EDGE_LOOP('',(#5392,#5393,#5394,#5395));
#1449=EDGE_LOOP('',(#5396,#5397,#5398,#5399));
#1450=EDGE_LOOP('',(#5400,#5401,#5402,#5403));
#1451=EDGE_LOOP('',(#5404,#5405,#5406,#5407));
#1452=EDGE_LOOP('',(#5408,#5409,#5410,#5411));
#1453=EDGE_LOOP('',(#5412,#5413,#5414,#5415));
#1454=EDGE_LOOP('',(#5416,#5417,#5418,#5419));
#1455=EDGE_LOOP('',(#5420,#5421,#5422,#5423));
#1456=EDGE_LOOP('',(#5424,#5425,#5426,#5427));
#1457=EDGE_LOOP('',(#5428,#5429,#5430,#5431));
#1458=EDGE_LOOP('',(#5432,#5433,#5434,#5435));
#1459=EDGE_LOOP('',(#5436,#5437,#5438,#5439));
#1460=EDGE_LOOP('',(#5440,#5441,#5442,#5443));
#1461=EDGE_LOOP('',(#5444,#5445,#5446,#5447));
#1462=EDGE_LOOP('',(#5448,#5449,#5450,#5451));
#1463=EDGE_LOOP('',(#5452,#5453,#5454,#5455));
#1464=EDGE_LOOP('',(#5456,#5457,#5458,#5459));
#1465=EDGE_LOOP('',(#5460,#5461,#5462,#5463));
#1466=EDGE_LOOP('',(#5464,#5465,#5466,#5467));
#1467=EDGE_LOOP('',(#5468,#5469,#5470,#5471));
#1468=EDGE_LOOP('',(#5472,#5473,#5474,#5475));
#1469=EDGE_LOOP('',(#5476,#5477,#5478,#5479));
#1470=EDGE_LOOP('',(#5480,#5481,#5482,#5483));
#1471=EDGE_LOOP('',(#5484,#5485,#5486,#5487));
#1472=EDGE_LOOP('',(#5488,#5489,#5490,#5491));
#1473=EDGE_LOOP('',(#5492,#5493,#5494,#5495));
#1474=EDGE_LOOP('',(#5496,#5497,#5498,#5499,#5500,#5501,#5502,#5503,#5504,
#5505,#5506,#5507,#5508,#5509,#5510,#5511,#5512,#5513,#5514,#5515,#5516,
#5517,#5518,#5519,#5520,#5521,#5522,#5523,#5524,#5525,#5526,#5527,#5528,
#5529,#5530,#5531,#5532,#5533,#5534,#5535,#5536,#5537,#5538,#5539));
#1475=EDGE_LOOP('',(#5540));
#1476=EDGE_LOOP('',(#5541,#5542,#5543,#5544,#5545,#5546,#5547,#5548,#5549,
#5550,#5551,#5552,#5553,#5554,#5555,#5556,#5557,#5558,#5559,#5560,#5561,
#5562,#5563,#5564,#5565,#5566,#5567,#5568,#5569,#5570,#5571,#5572,#5573,
#5574,#5575,#5576,#5577,#5578,#5579,#5580,#5581,#5582,#5583,#5584));
#1477=EDGE_LOOP('',(#5585));
#1478=EDGE_LOOP('',(#5586,#5587,#5588,#5589));
#1479=EDGE_LOOP('',(#5590));
#1480=EDGE_LOOP('',(#5591));
#1481=EDGE_LOOP('',(#5592,#5593,#5594,#5595));
#1482=EDGE_LOOP('',(#5596));
#1483=EDGE_LOOP('',(#5597));
#1484=EDGE_LOOP('',(#5598,#5599,#5600,#5601));
#1485=EDGE_LOOP('',(#5602));
#1486=EDGE_LOOP('',(#5603));
#1487=EDGE_LOOP('',(#5604,#5605,#5606,#5607));
#1488=EDGE_LOOP('',(#5608));
#1489=EDGE_LOOP('',(#5609));
#1490=EDGE_LOOP('',(#5610,#5611,#5612,#5613));
#1491=EDGE_LOOP('',(#5614,#5615,#5616,#5617));
#1492=EDGE_LOOP('',(#5618,#5619,#5620,#5621));
#1493=EDGE_LOOP('',(#5622,#5623,#5624,#5625));
#1494=EDGE_LOOP('',(#5626,#5627,#5628,#5629));
#1495=EDGE_LOOP('',(#5630,#5631,#5632,#5633));
#1496=EDGE_LOOP('',(#5634,#5635,#5636,#5637));
#1497=EDGE_LOOP('',(#5638,#5639,#5640,#5641));
#1498=EDGE_LOOP('',(#5642,#5643,#5644,#5645));
#1499=EDGE_LOOP('',(#5646));
#1500=EDGE_LOOP('',(#5647));
#1501=EDGE_LOOP('',(#5648));
#1502=EDGE_LOOP('',(#5649));
#1503=EDGE_LOOP('',(#5650,#5651,#5652,#5653));
#1504=EDGE_LOOP('',(#5654,#5655,#5656,#5657));
#1505=EDGE_LOOP('',(#5658,#5659,#5660,#5661));
#1506=EDGE_LOOP('',(#5662,#5663,#5664,#5665));
#1507=EDGE_LOOP('',(#5666,#5667,#5668,#5669));
#1508=EDGE_LOOP('',(#5670,#5671,#5672,#5673));
#1509=EDGE_LOOP('',(#5674));
#1510=EDGE_LOOP('',(#5675));
#1511=EDGE_LOOP('',(#5676));
#1512=EDGE_LOOP('',(#5677));
#1513=EDGE_LOOP('',(#5678,#5679,#5680,#5681));
#1514=EDGE_LOOP('',(#5682,#5683,#5684,#5685,#5686,#5687,#5688,#5689,#5690,
#5691,#5692,#5693));
#1515=EDGE_LOOP('',(#5694,#5695,#5696,#5697,#5698,#5699,#5700,#5701,#5702,
#5703,#5704,#5705));
#1516=EDGE_LOOP('',(#5706,#5707,#5708,#5709));
#1517=EDGE_LOOP('',(#5710,#5711,#5712,#5713));
#1518=EDGE_LOOP('',(#5714,#5715,#5716,#5717));
#1519=EDGE_LOOP('',(#5718,#5719,#5720,#5721));
#1520=EDGE_LOOP('',(#5722,#5723,#5724,#5725));
#1521=EDGE_LOOP('',(#5726,#5727,#5728,#5729));
#1522=EDGE_LOOP('',(#5730,#5731,#5732,#5733,#5734,#5735));
#1523=EDGE_LOOP('',(#5736,#5737,#5738,#5739,#5740,#5741));
#1524=EDGE_LOOP('',(#5742));
#1525=EDGE_LOOP('',(#5743));
#1526=EDGE_LOOP('',(#5744,#5745,#5746,#5747));
#1527=EDGE_LOOP('',(#5748));
#1528=EDGE_LOOP('',(#5749));
#1529=EDGE_LOOP('',(#5750,#5751,#5752,#5753));
#1530=EDGE_LOOP('',(#5754,#5755,#5756,#5757));
#1531=EDGE_LOOP('',(#5758,#5759,#5760,#5761));
#1532=EDGE_LOOP('',(#5762));
#1533=EDGE_LOOP('',(#5763));
#1534=EDGE_LOOP('',(#5764,#5765,#5766,#5767));
#1535=EDGE_LOOP('',(#5768,#5769,#5770,#5771));
#1536=EDGE_LOOP('',(#5772));
#1537=EDGE_LOOP('',(#5773,#5774,#5775,#5776));
#1538=EDGE_LOOP('',(#5777,#5778,#5779,#5780));
#1539=EDGE_LOOP('',(#5781,#5782,#5783,#5784));
#1540=EDGE_LOOP('',(#5785));
#1541=EDGE_LOOP('',(#5786));
#1542=EDGE_LOOP('',(#5787,#5788,#5789,#5790));
#1543=EDGE_LOOP('',(#5791,#5792,#5793,#5794));
#1544=EDGE_LOOP('',(#5795,#5796,#5797,#5798));
#1545=EDGE_LOOP('',(#5799));
#1546=EDGE_LOOP('',(#5800,#5801,#5802,#5803));
#1547=EDGE_LOOP('',(#5804,#5805,#5806,#5807));
#1548=EDGE_LOOP('',(#5808,#5809,#5810,#5811));
#1549=EDGE_LOOP('',(#5812,#5813,#5814,#5815));
#1550=EDGE_LOOP('',(#5816,#5817,#5818,#5819));
#1551=EDGE_LOOP('',(#5820,#5821,#5822,#5823));
#1552=EDGE_LOOP('',(#5824,#5825,#5826,#5827,#5828,#5829));
#1553=EDGE_LOOP('',(#5830,#5831,#5832,#5833,#5834,#5835));
#1554=EDGE_LOOP('',(#5836,#5837,#5838,#5839));
#1555=EDGE_LOOP('',(#5840,#5841,#5842,#5843));
#1556=EDGE_LOOP('',(#5844,#5845,#5846,#5847));
#1557=EDGE_LOOP('',(#5848));
#1558=EDGE_LOOP('',(#5849,#5850,#5851,#5852,#5853,#5854,#5855,#5856,#5857,
#5858));
#1559=EDGE_LOOP('',(#5859,#5860,#5861,#5862));
#1560=EDGE_LOOP('',(#5863,#5864,#5865,#5866));
#1561=EDGE_LOOP('',(#5867,#5868,#5869,#5870,#5871,#5872,#5873,#5874,#5875,
#5876));
#1562=EDGE_LOOP('',(#5877,#5878,#5879,#5880));
#1563=EDGE_LOOP('',(#5881,#5882,#5883,#5884,#5885,#5886));
#1564=EDGE_LOOP('',(#5887,#5888,#5889,#5890,#5891,#5892,#5893,#5894));
#1565=EDGE_LOOP('',(#5895,#5896,#5897,#5898,#5899));
#1566=EDGE_LOOP('',(#5900,#5901,#5902,#5903));
#1567=EDGE_LOOP('',(#5904,#5905,#5906,#5907,#5908,#5909));
#1568=EDGE_LOOP('',(#5910,#5911,#5912,#5913));
#1569=EDGE_LOOP('',(#5914,#5915,#5916,#5917));
#1570=EDGE_LOOP('',(#5918,#5919,#5920,#5921));
#1571=EDGE_LOOP('',(#5922));
#1572=EDGE_LOOP('',(#5923));
#1573=EDGE_LOOP('',(#5924,#5925,#5926,#5927));
#1574=EDGE_LOOP('',(#5928));
#1575=EDGE_LOOP('',(#5929));
#1576=EDGE_LOOP('',(#5930,#5931,#5932,#5933));
#1577=EDGE_LOOP('',(#5934,#5935,#5936,#5937));
#1578=EDGE_LOOP('',(#5938,#5939,#5940,#5941));
#1579=EDGE_LOOP('',(#5942,#5943,#5944,#5945));
#1580=EDGE_LOOP('',(#5946,#5947,#5948,#5949));
#1581=EDGE_LOOP('',(#5950,#5951,#5952,#5953,#5954,#5955));
#1582=EDGE_LOOP('',(#5956,#5957,#5958,#5959));
#1583=EDGE_LOOP('',(#5960,#5961,#5962,#5963));
#1584=EDGE_LOOP('',(#5964,#5965,#5966,#5967));
#1585=EDGE_LOOP('',(#5968,#5969,#5970,#5971));
#1586=EDGE_LOOP('',(#5972,#5973));
#1587=EDGE_LOOP('',(#5974,#5975,#5976,#5977,#5978,#5979,#5980,#5981,#5982,
#5983,#5984,#5985));
#1588=EDGE_LOOP('',(#5986));
#1589=EDGE_LOOP('',(#5987));
#1590=EDGE_LOOP('',(#5988));
#1591=EDGE_LOOP('',(#5989));
#1592=EDGE_LOOP('',(#5990));
#1593=EDGE_LOOP('',(#5991,#5992,#5993,#5994));
#1594=EDGE_LOOP('',(#5995,#5996,#5997,#5998,#5999,#6000,#6001,#6002,#6003,
#6004,#6005,#6006,#6007,#6008));
#1595=EDGE_LOOP('',(#6009));
#1596=EDGE_LOOP('',(#6010));
#1597=EDGE_LOOP('',(#6011));
#1598=EDGE_LOOP('',(#6012,#6013,#6014,#6015));
#1599=EDGE_LOOP('',(#6016,#6017,#6018,#6019));
#1600=EDGE_LOOP('',(#6020,#6021));
#1601=EDGE_LOOP('',(#6022,#6023,#6024,#6025));
#1602=EDGE_LOOP('',(#6026,#6027,#6028,#6029));
#1603=EDGE_LOOP('',(#6030,#6031,#6032,#6033));
#1604=EDGE_LOOP('',(#6034,#6035,#6036,#6037));
#1605=EDGE_LOOP('',(#6038,#6039,#6040,#6041));
#1606=EDGE_LOOP('',(#6042,#6043,#6044,#6045));
#1607=EDGE_LOOP('',(#6046,#6047,#6048,#6049));
#1608=EDGE_LOOP('',(#6050,#6051,#6052,#6053,#6054,#6055));
#1609=EDGE_LOOP('',(#6056));
#1610=EDGE_LOOP('',(#6057));
#1611=EDGE_LOOP('',(#6058));
#1612=EDGE_LOOP('',(#6059,#6060,#6061,#6062));
#1613=EDGE_LOOP('',(#6063,#6064,#6065,#6066,#6067,#6068,#6069,#6070));
#1614=EDGE_LOOP('',(#6071));
#1615=EDGE_LOOP('',(#6072));
#1616=EDGE_LOOP('',(#6073));
#1617=EDGE_LOOP('',(#6074));
#1618=EDGE_LOOP('',(#6075));
#1619=EDGE_LOOP('',(#6076,#6077,#6078,#6079,#6080,#6081));
#1620=EDGE_LOOP('',(#6082,#6083,#6084,#6085));
#1621=EDGE_LOOP('',(#6086,#6087,#6088,#6089));
#1622=EDGE_LOOP('',(#6090,#6091,#6092,#6093));
#1623=EDGE_LOOP('',(#6094,#6095,#6096,#6097));
#1624=EDGE_LOOP('',(#6098));
#1625=EDGE_LOOP('',(#6099));
#1626=EDGE_LOOP('',(#6100));
#1627=EDGE_LOOP('',(#6101));
#1628=EDGE_LOOP('',(#6102,#6103,#6104,#6105));
#1629=EDGE_LOOP('',(#6106));
#1630=EDGE_LOOP('',(#6107,#6108,#6109,#6110));
#1631=EDGE_LOOP('',(#6111));
#1632=EDGE_LOOP('',(#6112));
#1633=EDGE_LOOP('',(#6113));
#1634=EDGE_LOOP('',(#6114,#6115,#6116,#6117));
#1635=EDGE_LOOP('',(#6118));
#1636=EDGE_LOOP('',(#6119));
#1637=EDGE_LOOP('',(#6120,#6121,#6122,#6123));
#1638=EDGE_LOOP('',(#6124));
#1639=EDGE_LOOP('',(#6125));
#1640=EDGE_LOOP('',(#6126,#6127,#6128,#6129));
#1641=EDGE_LOOP('',(#6130,#6131,#6132,#6133));
#1642=EDGE_LOOP('',(#6134));
#1643=EDGE_LOOP('',(#6135));
#1644=EDGE_LOOP('',(#6136));
#1645=EDGE_LOOP('',(#6137));
#1646=EDGE_LOOP('',(#6138,#6139,#6140,#6141));
#1647=EDGE_LOOP('',(#6142,#6143,#6144,#6145));
#1648=EDGE_LOOP('',(#6146));
#1649=EDGE_LOOP('',(#6147,#6148,#6149,#6150));
#1650=EDGE_LOOP('',(#6151));
#1651=EDGE_LOOP('',(#6152,#6153,#6154,#6155));
#1652=EDGE_LOOP('',(#6156,#6157,#6158,#6159));
#1653=EDGE_LOOP('',(#6160));
#1654=EDGE_LOOP('',(#6161,#6162,#6163,#6164));
#1655=EDGE_LOOP('',(#6165));
#1656=EDGE_LOOP('',(#6166,#6167,#6168,#6169));
#1657=EDGE_LOOP('',(#6170,#6171,#6172,#6173));
#1658=EDGE_LOOP('',(#6174,#6175,#6176,#6177));
#1659=EDGE_LOOP('',(#6178,#6179,#6180,#6181));
#1660=EDGE_LOOP('',(#6182,#6183,#6184,#6185));
#1661=EDGE_LOOP('',(#6186,#6187,#6188,#6189));
#1662=EDGE_LOOP('',(#6190,#6191,#6192,#6193));
#1663=EDGE_LOOP('',(#6194,#6195,#6196,#6197));
#1664=EDGE_LOOP('',(#6198,#6199,#6200,#6201));
#1665=EDGE_LOOP('',(#6202));
#1666=EDGE_LOOP('',(#6203));
#1667=EDGE_LOOP('',(#6204));
#1668=EDGE_LOOP('',(#6205,#6206,#6207,#6208));
#1669=EDGE_LOOP('',(#6209));
#1670=EDGE_LOOP('',(#6210,#6211));
#1671=EDGE_LOOP('',(#6212,#6213,#6214,#6215,#6216,#6217,#6218,#6219));
#1672=EDGE_LOOP('',(#6220,#6221));
#1673=EDGE_LOOP('',(#6222,#6223,#6224,#6225,#6226,#6227,#6228,#6229));
#1674=EDGE_LOOP('',(#6230,#6231));
#1675=EDGE_LOOP('',(#6232,#6233,#6234,#6235,#6236,#6237,#6238,#6239));
#1676=EDGE_LOOP('',(#6240,#6241));
#1677=EDGE_LOOP('',(#6242,#6243,#6244,#6245,#6246,#6247,#6248,#6249));
#1678=EDGE_LOOP('',(#6250,#6251,#6252,#6253,#6254,#6255,#6256,#6257,#6258,
#6259,#6260,#6261));
#1679=EDGE_LOOP('',(#6262,#6263,#6264,#6265,#6266,#6267,#6268,#6269,#6270,
#6271,#6272,#6273));
#1680=EDGE_LOOP('',(#6274,#6275,#6276,#6277,#6278,#6279,#6280,#6281,#6282,
#6283,#6284,#6285));
#1681=EDGE_LOOP('',(#6286,#6287,#6288,#6289,#6290,#6291,#6292,#6293,#6294,
#6295));
#1682=EDGE_LOOP('',(#6296,#6297,#6298,#6299));
#1683=EDGE_LOOP('',(#6300,#6301,#6302,#6303));
#1684=EDGE_LOOP('',(#6304));
#1685=EDGE_LOOP('',(#6305));
#1686=EDGE_LOOP('',(#6306));
#1687=EDGE_LOOP('',(#6307));
#1688=EDGE_LOOP('',(#6308,#6309,#6310,#6311));
#1689=EDGE_LOOP('',(#6312,#6313,#6314,#6315,#6316,#6317,#6318,#6319,#6320,
#6321));
#1690=EDGE_LOOP('',(#6322,#6323,#6324,#6325));
#1691=EDGE_LOOP('',(#6326,#6327,#6328,#6329));
#1692=EDGE_LOOP('',(#6330,#6331,#6332,#6333));
#1693=EDGE_LOOP('',(#6334,#6335,#6336,#6337));
#1694=EDGE_LOOP('',(#6338,#6339,#6340,#6341));
#1695=EDGE_LOOP('',(#6342,#6343,#6344,#6345,#6346,#6347,#6348,#6349,#6350,
#6351,#6352,#6353));
#1696=EDGE_LOOP('',(#6354,#6355,#6356,#6357));
#1697=EDGE_LOOP('',(#6358,#6359,#6360,#6361));
#1698=EDGE_LOOP('',(#6362,#6363,#6364,#6365));
#1699=EDGE_LOOP('',(#6366,#6367,#6368,#6369));
#1700=EDGE_LOOP('',(#6370,#6371,#6372,#6373));
#1701=EDGE_LOOP('',(#6374,#6375,#6376,#6377));
#1702=EDGE_LOOP('',(#6378,#6379,#6380,#6381));
#1703=EDGE_LOOP('',(#6382,#6383,#6384,#6385));
#1704=EDGE_LOOP('',(#6386,#6387,#6388,#6389,#6390,#6391,#6392,#6393));
#1705=EDGE_LOOP('',(#6394,#6395,#6396,#6397,#6398,#6399,#6400,#6401));
#1706=EDGE_LOOP('',(#6402,#6403,#6404,#6405));
#1707=EDGE_LOOP('',(#6406,#6407,#6408,#6409));
#1708=EDGE_LOOP('',(#6410,#6411,#6412,#6413));
#1709=EDGE_LOOP('',(#6414,#6415,#6416,#6417));
#1710=EDGE_LOOP('',(#6418,#6419,#6420,#6421));
#1711=EDGE_LOOP('',(#6422,#6423,#6424,#6425));
#1712=EDGE_LOOP('',(#6426,#6427,#6428,#6429));
#1713=EDGE_LOOP('',(#6430,#6431,#6432,#6433));
#1714=EDGE_LOOP('',(#6434,#6435,#6436,#6437,#6438,#6439,#6440,#6441));
#1715=EDGE_LOOP('',(#6442,#6443,#6444,#6445,#6446,#6447,#6448,#6449));
#1716=EDGE_LOOP('',(#6450,#6451,#6452,#6453));
#1717=EDGE_LOOP('',(#6454,#6455,#6456,#6457));
#1718=EDGE_LOOP('',(#6458,#6459,#6460,#6461));
#1719=EDGE_LOOP('',(#6462,#6463,#6464,#6465));
#1720=EDGE_LOOP('',(#6466,#6467,#6468,#6469));
#1721=EDGE_LOOP('',(#6470,#6471,#6472,#6473));
#1722=EDGE_LOOP('',(#6474,#6475,#6476,#6477,#6478,#6479));
#1723=EDGE_LOOP('',(#6480,#6481,#6482,#6483,#6484,#6485));
#1724=EDGE_LOOP('',(#6486));
#1725=EDGE_LOOP('',(#6487));
#1726=EDGE_LOOP('',(#6488,#6489,#6490,#6491));
#1727=EDGE_LOOP('',(#6492,#6493,#6494,#6495));
#1728=EDGE_LOOP('',(#6496,#6497,#6498,#6499));
#1729=EDGE_LOOP('',(#6500));
#1730=EDGE_LOOP('',(#6501));
#1731=EDGE_LOOP('',(#6502,#6503,#6504,#6505));
#1732=EDGE_LOOP('',(#6506,#6507,#6508,#6509));
#1733=EDGE_LOOP('',(#6510));
#1734=EDGE_LOOP('',(#6511,#6512,#6513,#6514));
#1735=EDGE_LOOP('',(#6515,#6516,#6517,#6518));
#1736=EDGE_LOOP('',(#6519,#6520,#6521,#6522));
#1737=EDGE_LOOP('',(#6523));
#1738=EDGE_LOOP('',(#6524));
#1739=EDGE_LOOP('',(#6525,#6526,#6527,#6528));
#1740=EDGE_LOOP('',(#6529,#6530,#6531,#6532));
#1741=EDGE_LOOP('',(#6533,#6534,#6535,#6536));
#1742=EDGE_LOOP('',(#6537));
#1743=EDGE_LOOP('',(#6538,#6539,#6540,#6541));
#1744=EDGE_LOOP('',(#6542,#6543,#6544,#6545));
#1745=EDGE_LOOP('',(#6546,#6547,#6548,#6549));
#1746=EDGE_LOOP('',(#6550,#6551,#6552,#6553));
#1747=EDGE_LOOP('',(#6554,#6555,#6556,#6557));
#1748=EDGE_LOOP('',(#6558,#6559,#6560,#6561));
#1749=EDGE_LOOP('',(#6562,#6563,#6564,#6565,#6566,#6567));
#1750=EDGE_LOOP('',(#6568,#6569,#6570,#6571,#6572,#6573));
#1751=LINE('',#10345,#2422);
#1752=LINE('',#10352,#2423);
#1753=LINE('',#10359,#2424);
#1754=LINE('',#10366,#2425);
#1755=LINE('',#10373,#2426);
#1756=LINE('',#10378,#2427);
#1757=LINE('',#10380,#2428);
#1758=LINE('',#10382,#2429);
#1759=LINE('',#10383,#2430);
#1760=LINE('',#10386,#2431);
#1761=LINE('',#10388,#2432);
#1762=LINE('',#10389,#2433);
#1763=LINE('',#10392,#2434);
#1764=LINE('',#10394,#2435);
#1765=LINE('',#10395,#2436);
#1766=LINE('',#10397,#2437);
#1767=LINE('',#10398,#2438);
#1768=LINE('',#10405,#2439);
#1769=LINE('',#10407,#2440);
#1770=LINE('',#10409,#2441);
#1771=LINE('',#10410,#2442);
#1772=LINE('',#10413,#2443);
#1773=LINE('',#10415,#2444);
#1774=LINE('',#10416,#2445);
#1775=LINE('',#10419,#2446);
#1776=LINE('',#10421,#2447);
#1777=LINE('',#10422,#2448);
#1778=LINE('',#10424,#2449);
#1779=LINE('',#10425,#2450);
#1780=LINE('',#10432,#2451);
#1781=LINE('',#10434,#2452);
#1782=LINE('',#10436,#2453);
#1783=LINE('',#10437,#2454);
#1784=LINE('',#10440,#2455);
#1785=LINE('',#10442,#2456);
#1786=LINE('',#10443,#2457);
#1787=LINE('',#10446,#2458);
#1788=LINE('',#10448,#2459);
#1789=LINE('',#10449,#2460);
#1790=LINE('',#10451,#2461);
#1791=LINE('',#10452,#2462);
#1792=LINE('',#10460,#2463);
#1793=LINE('',#10465,#2464);
#1794=LINE('',#10467,#2465);
#1795=LINE('',#10469,#2466);
#1796=LINE('',#10470,#2467);
#1797=LINE('',#10473,#2468);
#1798=LINE('',#10475,#2469);
#1799=LINE('',#10476,#2470);
#1800=LINE('',#10479,#2471);
#1801=LINE('',#10481,#2472);
#1802=LINE('',#10482,#2473);
#1803=LINE('',#10484,#2474);
#1804=LINE('',#10485,#2475);
#1805=LINE('',#10493,#2476);
#1806=LINE('',#10499,#2477);
#1807=LINE('',#10505,#2478);
#1808=LINE('',#10511,#2479);
#1809=LINE('',#10517,#2480);
#1810=LINE('',#10523,#2481);
#1811=LINE('',#10529,#2482);
#1812=LINE('',#10535,#2483);
#1813=LINE('',#10540,#2484);
#1814=LINE('',#10542,#2485);
#1815=LINE('',#10544,#2486);
#1816=LINE('',#10545,#2487);
#1817=LINE('',#10549,#2488);
#1818=LINE('',#10551,#2489);
#1819=LINE('',#10553,#2490);
#1820=LINE('',#10554,#2491);
#1821=LINE('',#10556,#2492);
#1822=LINE('',#10557,#2493);
#1823=LINE('',#10560,#2494);
#1824=LINE('',#10562,#2495);
#1825=LINE('',#10564,#2496);
#1826=LINE('',#10566,#2497);
#1827=LINE('',#10567,#2498);
#1828=LINE('',#10570,#2499);
#1829=LINE('',#10571,#2500);
#1830=LINE('',#10574,#2501);
#1831=LINE('',#10575,#2502);
#1832=LINE('',#10578,#2503);
#1833=LINE('',#10580,#2504);
#1834=LINE('',#10581,#2505);
#1835=LINE('',#10583,#2506);
#1836=LINE('',#10584,#2507);
#1837=LINE('',#10592,#2508);
#1838=LINE('',#10597,#2509);
#1839=LINE('',#10599,#2510);
#1840=LINE('',#10601,#2511);
#1841=LINE('',#10602,#2512);
#1842=LINE('',#10605,#2513);
#1843=LINE('',#10607,#2514);
#1844=LINE('',#10608,#2515);
#1845=LINE('',#10611,#2516);
#1846=LINE('',#10613,#2517);
#1847=LINE('',#10614,#2518);
#1848=LINE('',#10616,#2519);
#1849=LINE('',#10617,#2520);
#1850=LINE('',#10625,#2521);
#1851=LINE('',#10630,#2522);
#1852=LINE('',#10632,#2523);
#1853=LINE('',#10634,#2524);
#1854=LINE('',#10635,#2525);
#1855=LINE('',#10638,#2526);
#1856=LINE('',#10640,#2527);
#1857=LINE('',#10641,#2528);
#1858=LINE('',#10644,#2529);
#1859=LINE('',#10646,#2530);
#1860=LINE('',#10647,#2531);
#1861=LINE('',#10649,#2532);
#1862=LINE('',#10650,#2533);
#1863=LINE('',#10658,#2534);
#1864=LINE('',#10664,#2535);
#1865=LINE('',#10670,#2536);
#1866=LINE('',#10676,#2537);
#1867=LINE('',#10684,#2538);
#1868=LINE('',#10693,#2539);
#1869=LINE('',#10699,#2540);
#1870=LINE('',#10708,#2541);
#1871=LINE('',#10714,#2542);
#1872=LINE('',#10720,#2543);
#1873=LINE('',#10729,#2544);
#1874=LINE('',#10735,#2545);
#1875=LINE('',#10740,#2546);
#1876=LINE('',#10756,#2547);
#1877=LINE('',#10759,#2548);
#1878=LINE('',#10764,#2549);
#1879=LINE('',#10772,#2550);
#1880=LINE('',#10778,#2551);
#1881=LINE('',#10794,#2552);
#1882=LINE('',#10797,#2553);
#1883=LINE('',#10802,#2554);
#1884=LINE('',#10810,#2555);
#1885=LINE('',#10816,#2556);
#1886=LINE('',#13475,#2557);
#1887=LINE('',#13480,#2558);
#1888=LINE('',#13484,#2559);
#1889=LINE('',#13486,#2560);
#1890=LINE('',#13488,#2561);
#1891=LINE('',#13489,#2562);
#1892=LINE('',#13493,#2563);
#1893=LINE('',#13497,#2564);
#1894=LINE('',#13507,#2565);
#1895=LINE('',#13510,#2566);
#1896=LINE('',#13512,#2567);
#1897=LINE('',#13513,#2568);
#1898=LINE('',#13515,#2569);
#1899=LINE('',#13516,#2570);
#1900=LINE('',#13527,#2571);
#1901=LINE('',#13532,#2572);
#1902=LINE('',#13536,#2573);
#1903=LINE('',#13538,#2574);
#1904=LINE('',#13540,#2575);
#1905=LINE('',#13541,#2576);
#1906=LINE('',#13545,#2577);
#1907=LINE('',#13550,#2578);
#1908=LINE('',#13559,#2579);
#1909=LINE('',#13562,#2580);
#1910=LINE('',#13564,#2581);
#1911=LINE('',#13565,#2582);
#1912=LINE('',#13567,#2583);
#1913=LINE('',#13568,#2584);
#1914=LINE('',#13575,#2585);
#1915=LINE('',#13577,#2586);
#1916=LINE('',#13579,#2587);
#1917=LINE('',#13580,#2588);
#1918=LINE('',#13583,#2589);
#1919=LINE('',#13585,#2590);
#1920=LINE('',#13586,#2591);
#1921=LINE('',#13589,#2592);
#1922=LINE('',#13591,#2593);
#1923=LINE('',#13592,#2594);
#1924=LINE('',#13595,#2595);
#1925=LINE('',#13597,#2596);
#1926=LINE('',#13598,#2597);
#1927=LINE('',#13601,#2598);
#1928=LINE('',#13603,#2599);
#1929=LINE('',#13604,#2600);
#1930=LINE('',#13607,#2601);
#1931=LINE('',#13609,#2602);
#1932=LINE('',#13610,#2603);
#1933=LINE('',#13613,#2604);
#1934=LINE('',#13615,#2605);
#1935=LINE('',#13616,#2606);
#1936=LINE('',#13619,#2607);
#1937=LINE('',#13621,#2608);
#1938=LINE('',#13622,#2609);
#1939=LINE('',#13625,#2610);
#1940=LINE('',#13627,#2611);
#1941=LINE('',#13628,#2612);
#1942=LINE('',#13632,#2613);
#1943=LINE('',#13634,#2614);
#1944=LINE('',#13636,#2615);
#1945=LINE('',#13637,#2616);
#1946=LINE('',#13640,#2617);
#1947=LINE('',#13642,#2618);
#1948=LINE('',#13643,#2619);
#1949=LINE('',#13646,#2620);
#1950=LINE('',#13648,#2621);
#1951=LINE('',#13649,#2622);
#1952=LINE('',#13652,#2623);
#1953=LINE('',#13654,#2624);
#1954=LINE('',#13655,#2625);
#1955=LINE('',#13658,#2626);
#1956=LINE('',#13660,#2627);
#1957=LINE('',#13661,#2628);
#1958=LINE('',#13664,#2629);
#1959=LINE('',#13666,#2630);
#1960=LINE('',#13667,#2631);
#1961=LINE('',#13670,#2632);
#1962=LINE('',#13672,#2633);
#1963=LINE('',#13673,#2634);
#1964=LINE('',#13676,#2635);
#1965=LINE('',#13678,#2636);
#1966=LINE('',#13679,#2637);
#1967=LINE('',#13682,#2638);
#1968=LINE('',#13684,#2639);
#1969=LINE('',#13685,#2640);
#1970=LINE('',#13689,#2641);
#1971=LINE('',#13691,#2642);
#1972=LINE('',#13693,#2643);
#1973=LINE('',#13694,#2644);
#1974=LINE('',#13697,#2645);
#1975=LINE('',#13699,#2646);
#1976=LINE('',#13700,#2647);
#1977=LINE('',#13703,#2648);
#1978=LINE('',#13705,#2649);
#1979=LINE('',#13706,#2650);
#1980=LINE('',#13709,#2651);
#1981=LINE('',#13711,#2652);
#1982=LINE('',#13712,#2653);
#1983=LINE('',#13715,#2654);
#1984=LINE('',#13717,#2655);
#1985=LINE('',#13718,#2656);
#1986=LINE('',#13721,#2657);
#1987=LINE('',#13723,#2658);
#1988=LINE('',#13724,#2659);
#1989=LINE('',#13727,#2660);
#1990=LINE('',#13729,#2661);
#1991=LINE('',#13730,#2662);
#1992=LINE('',#13733,#2663);
#1993=LINE('',#13735,#2664);
#1994=LINE('',#13736,#2665);
#1995=LINE('',#13739,#2666);
#1996=LINE('',#13741,#2667);
#1997=LINE('',#13742,#2668);
#1998=LINE('',#13746,#2669);
#1999=LINE('',#13748,#2670);
#2000=LINE('',#13750,#2671);
#2001=LINE('',#13751,#2672);
#2002=LINE('',#13754,#2673);
#2003=LINE('',#13756,#2674);
#2004=LINE('',#13757,#2675);
#2005=LINE('',#13760,#2676);
#2006=LINE('',#13762,#2677);
#2007=LINE('',#13763,#2678);
#2008=LINE('',#13766,#2679);
#2009=LINE('',#13768,#2680);
#2010=LINE('',#13769,#2681);
#2011=LINE('',#13772,#2682);
#2012=LINE('',#13774,#2683);
#2013=LINE('',#13775,#2684);
#2014=LINE('',#13778,#2685);
#2015=LINE('',#13780,#2686);
#2016=LINE('',#13781,#2687);
#2017=LINE('',#13784,#2688);
#2018=LINE('',#13786,#2689);
#2019=LINE('',#13787,#2690);
#2020=LINE('',#13790,#2691);
#2021=LINE('',#13792,#2692);
#2022=LINE('',#13793,#2693);
#2023=LINE('',#13796,#2694);
#2024=LINE('',#13798,#2695);
#2025=LINE('',#13799,#2696);
#2026=LINE('',#13804,#2697);
#2027=LINE('',#13808,#2698);
#2028=LINE('',#13810,#2699);
#2029=LINE('',#13811,#2700);
#2030=LINE('',#13814,#2701);
#2031=LINE('',#13816,#2702);
#2032=LINE('',#13817,#2703);
#2033=LINE('',#13819,#2704);
#2034=LINE('',#13820,#2705);
#2035=LINE('',#13823,#2706);
#2036=LINE('',#13825,#2707);
#2037=LINE('',#13826,#2708);
#2038=LINE('',#13828,#2709);
#2039=LINE('',#13829,#2710);
#2040=LINE('',#13832,#2711);
#2041=LINE('',#13834,#2712);
#2042=LINE('',#13835,#2713);
#2043=LINE('',#13837,#2714);
#2044=LINE('',#13838,#2715);
#2045=LINE('',#13840,#2716);
#2046=LINE('',#13841,#2717);
#2047=LINE('',#13849,#2718);
#2048=LINE('',#13858,#2719);
#2049=LINE('',#13867,#2720);
#2050=LINE('',#13876,#2721);
#2051=LINE('',#13884,#2722);
#2052=LINE('',#13888,#2723);
#2053=LINE('',#13892,#2724);
#2054=LINE('',#13896,#2725);
#2055=LINE('',#13900,#2726);
#2056=LINE('',#13902,#2727);
#2057=LINE('',#13904,#2728);
#2058=LINE('',#13905,#2729);
#2059=LINE('',#13908,#2730);
#2060=LINE('',#13910,#2731);
#2061=LINE('',#13911,#2732);
#2062=LINE('',#13914,#2733);
#2063=LINE('',#13916,#2734);
#2064=LINE('',#13917,#2735);
#2065=LINE('',#13920,#2736);
#2066=LINE('',#13922,#2737);
#2067=LINE('',#13923,#2738);
#2068=LINE('',#13926,#2739);
#2069=LINE('',#13928,#2740);
#2070=LINE('',#13929,#2741);
#2071=LINE('',#13932,#2742);
#2072=LINE('',#13934,#2743);
#2073=LINE('',#13935,#2744);
#2074=LINE('',#13938,#2745);
#2075=LINE('',#13940,#2746);
#2076=LINE('',#13941,#2747);
#2077=LINE('',#13944,#2748);
#2078=LINE('',#13946,#2749);
#2079=LINE('',#13947,#2750);
#2080=LINE('',#13950,#2751);
#2081=LINE('',#13952,#2752);
#2082=LINE('',#13953,#2753);
#2083=LINE('',#13956,#2754);
#2084=LINE('',#13958,#2755);
#2085=LINE('',#13959,#2756);
#2086=LINE('',#13962,#2757);
#2087=LINE('',#13964,#2758);
#2088=LINE('',#13965,#2759);
#2089=LINE('',#13967,#2760);
#2090=LINE('',#13968,#2761);
#2091=LINE('',#13975,#2762);
#2092=LINE('',#13977,#2763);
#2093=LINE('',#13979,#2764);
#2094=LINE('',#13980,#2765);
#2095=LINE('',#13983,#2766);
#2096=LINE('',#13985,#2767);
#2097=LINE('',#13986,#2768);
#2098=LINE('',#13989,#2769);
#2099=LINE('',#13991,#2770);
#2100=LINE('',#13992,#2771);
#2101=LINE('',#13995,#2772);
#2102=LINE('',#13997,#2773);
#2103=LINE('',#13998,#2774);
#2104=LINE('',#14001,#2775);
#2105=LINE('',#14003,#2776);
#2106=LINE('',#14004,#2777);
#2107=LINE('',#14006,#2778);
#2108=LINE('',#14007,#2779);
#2109=LINE('',#14017,#2780);
#2110=LINE('',#14026,#2781);
#2111=LINE('',#14030,#2782);
#2112=LINE('',#14034,#2783);
#2113=LINE('',#14041,#2784);
#2114=LINE('',#14043,#2785);
#2115=LINE('',#14051,#2786);
#2116=LINE('',#14055,#2787);
#2117=LINE('',#14059,#2788);
#2118=LINE('',#14066,#2789);
#2119=LINE('',#14070,#2790);
#2120=LINE('',#14074,#2791);
#2121=LINE('',#14079,#2792);
#2122=LINE('',#14081,#2793);
#2123=LINE('',#14083,#2794);
#2124=LINE('',#14084,#2795);
#2125=LINE('',#14087,#2796);
#2126=LINE('',#14089,#2797);
#2127=LINE('',#14090,#2798);
#2128=LINE('',#14093,#2799);
#2129=LINE('',#14095,#2800);
#2130=LINE('',#14096,#2801);
#2131=LINE('',#14099,#2802);
#2132=LINE('',#14101,#2803);
#2133=LINE('',#14102,#2804);
#2134=LINE('',#14105,#2805);
#2135=LINE('',#14107,#2806);
#2136=LINE('',#14108,#2807);
#2137=LINE('',#14110,#2808);
#2138=LINE('',#14111,#2809);
#2139=LINE('',#14118,#2810);
#2140=LINE('',#14120,#2811);
#2141=LINE('',#14122,#2812);
#2142=LINE('',#14123,#2813);
#2143=LINE('',#14126,#2814);
#2144=LINE('',#14128,#2815);
#2145=LINE('',#14129,#2816);
#2146=LINE('',#14132,#2817);
#2147=LINE('',#14134,#2818);
#2148=LINE('',#14135,#2819);
#2149=LINE('',#14140,#2820);
#2150=LINE('',#14142,#2821);
#2151=LINE('',#14144,#2822);
#2152=LINE('',#14146,#2823);
#2153=LINE('',#14148,#2824);
#2154=LINE('',#14150,#2825);
#2155=LINE('',#14151,#2826);
#2156=LINE('',#14154,#2827);
#2157=LINE('',#14155,#2828);
#2158=LINE('',#14158,#2829);
#2159=LINE('',#14159,#2830);
#2160=LINE('',#14162,#2831);
#2161=LINE('',#14164,#2832);
#2162=LINE('',#14166,#2833);
#2163=LINE('',#14168,#2834);
#2164=LINE('',#14169,#2835);
#2165=LINE('',#14171,#2836);
#2166=LINE('',#14174,#2837);
#2167=LINE('',#14177,#2838);
#2168=LINE('',#14181,#2839);
#2169=LINE('',#14188,#2840);
#2170=LINE('',#14190,#2841);
#2171=LINE('',#14192,#2842);
#2172=LINE('',#14199,#2843);
#2173=LINE('',#14203,#2844);
#2174=LINE('',#14210,#2845);
#2175=LINE('',#14219,#2846);
#2176=LINE('',#14224,#2847);
#2177=LINE('',#14226,#2848);
#2178=LINE('',#14228,#2849);
#2179=LINE('',#14229,#2850);
#2180=LINE('',#14232,#2851);
#2181=LINE('',#14234,#2852);
#2182=LINE('',#14235,#2853);
#2183=LINE('',#14239,#2854);
#2184=LINE('',#14240,#2855);
#2185=LINE('',#14241,#2856);
#2186=LINE('',#14244,#2857);
#2187=LINE('',#14246,#2858);
#2188=LINE('',#14247,#2859);
#2189=LINE('',#14250,#2860);
#2190=LINE('',#14252,#2861);
#2191=LINE('',#14254,#2862);
#2192=LINE('',#14256,#2863);
#2193=LINE('',#14257,#2864);
#2194=LINE('',#14262,#2865);
#2195=LINE('',#14268,#2866);
#2196=LINE('',#14274,#2867);
#2197=LINE('',#14279,#2868);
#2198=LINE('',#14283,#2869);
#2199=LINE('',#14286,#2870);
#2200=LINE('',#14289,#2871);
#2201=LINE('',#14291,#2872);
#2202=LINE('',#14293,#2873);
#2203=LINE('',#14296,#2874);
#2204=LINE('',#14297,#2875);
#2205=LINE('',#14308,#2876);
#2206=LINE('',#14312,#2877);
#2207=LINE('',#14314,#2878);
#2208=LINE('',#14315,#2879);
#2209=LINE('',#14317,#2880);
#2210=LINE('',#14319,#2881);
#2211=LINE('',#14321,#2882);
#2212=LINE('',#14323,#2883);
#2213=LINE('',#14324,#2884);
#2214=LINE('',#14327,#2885);
#2215=LINE('',#14334,#2886);
#2216=LINE('',#14338,#2887);
#2217=LINE('',#14342,#2888);
#2218=LINE('',#14344,#2889);
#2219=LINE('',#14345,#2890);
#2220=LINE('',#14348,#2891);
#2221=LINE('',#14349,#2892);
#2222=LINE('',#14352,#2893);
#2223=LINE('',#14353,#2894);
#2224=LINE('',#14356,#2895);
#2225=LINE('',#14357,#2896);
#2226=LINE('',#14359,#2897);
#2227=LINE('',#14361,#2898);
#2228=LINE('',#14364,#2899);
#2229=LINE('',#14365,#2900);
#2230=LINE('',#14368,#2901);
#2231=LINE('',#14370,#2902);
#2232=LINE('',#14371,#2903);
#2233=LINE('',#14373,#2904);
#2234=LINE('',#14374,#2905);
#2235=LINE('',#14382,#2906);
#2236=LINE('',#14388,#2907);
#2237=LINE('',#14397,#2908);
#2238=LINE('',#14404,#2909);
#2239=LINE('',#14415,#2910);
#2240=LINE('',#14419,#2911);
#2241=LINE('',#14427,#2912);
#2242=LINE('',#14433,#2913);
#2243=LINE('',#14442,#2914);
#2244=LINE('',#14448,#2915);
#2245=LINE('',#14454,#2916);
#2246=LINE('',#14456,#2917);
#2247=LINE('',#14458,#2918);
#2248=LINE('',#14459,#2919);
#2249=LINE('',#14462,#2920);
#2250=LINE('',#14464,#2921);
#2251=LINE('',#14465,#2922);
#2252=LINE('',#14468,#2923);
#2253=LINE('',#14470,#2924);
#2254=LINE('',#14471,#2925);
#2255=LINE('',#14473,#2926);
#2256=LINE('',#14474,#2927);
#2257=LINE('',#14481,#2928);
#2258=LINE('',#14483,#2929);
#2259=LINE('',#14485,#2930);
#2260=LINE('',#14486,#2931);
#2261=LINE('',#14489,#2932);
#2262=LINE('',#14491,#2933);
#2263=LINE('',#14492,#2934);
#2264=LINE('',#14495,#2935);
#2265=LINE('',#14497,#2936);
#2266=LINE('',#14498,#2937);
#2267=LINE('',#14500,#2938);
#2268=LINE('',#14501,#2939);
#2269=LINE('',#14509,#2940);
#2270=LINE('',#14517,#2941);
#2271=LINE('',#14525,#2942);
#2272=LINE('',#14529,#2943);
#2273=LINE('',#14533,#2944);
#2274=LINE('',#14537,#2945);
#2275=LINE('',#14541,#2946);
#2276=LINE('',#14545,#2947);
#2277=LINE('',#14549,#2948);
#2278=LINE('',#14553,#2949);
#2279=LINE('',#14557,#2950);
#2280=LINE('',#14561,#2951);
#2281=LINE('',#14565,#2952);
#2282=LINE('',#14569,#2953);
#2283=LINE('',#14573,#2954);
#2284=LINE('',#14577,#2955);
#2285=LINE('',#14581,#2956);
#2286=LINE('',#14585,#2957);
#2287=LINE('',#14587,#2958);
#2288=LINE('',#14589,#2959);
#2289=LINE('',#14591,#2960);
#2290=LINE('',#14593,#2961);
#2291=LINE('',#14595,#2962);
#2292=LINE('',#14596,#2963);
#2293=LINE('',#14598,#2964);
#2294=LINE('',#14600,#2965);
#2295=LINE('',#14602,#2966);
#2296=LINE('',#14604,#2967);
#2297=LINE('',#14606,#2968);
#2298=LINE('',#14607,#2969);
#2299=LINE('',#14610,#2970);
#2300=LINE('',#14612,#2971);
#2301=LINE('',#14614,#2972);
#2302=LINE('',#14616,#2973);
#2303=LINE('',#14617,#2974);
#2304=LINE('',#14619,#2975);
#2305=LINE('',#14621,#2976);
#2306=LINE('',#14623,#2977);
#2307=LINE('',#14625,#2978);
#2308=LINE('',#14626,#2979);
#2309=LINE('',#14629,#2980);
#2310=LINE('',#14630,#2981);
#2311=LINE('',#14633,#2982);
#2312=LINE('',#14634,#2983);
#2313=LINE('',#14637,#2984);
#2314=LINE('',#14638,#2985);
#2315=LINE('',#14641,#2986);
#2316=LINE('',#14642,#2987);
#2317=LINE('',#14644,#2988);
#2318=LINE('',#14647,#2989);
#2319=LINE('',#14648,#2990);
#2320=LINE('',#14651,#2991);
#2321=LINE('',#14652,#2992);
#2322=LINE('',#14655,#2993);
#2323=LINE('',#14656,#2994);
#2324=LINE('',#14659,#2995);
#2325=LINE('',#14660,#2996);
#2326=LINE('',#14662,#2997);
#2327=LINE('',#14668,#2998);
#2328=LINE('',#14670,#2999);
#2329=LINE('',#14672,#3000);
#2330=LINE('',#14673,#3001);
#2331=LINE('',#14676,#3002);
#2332=LINE('',#14678,#3003);
#2333=LINE('',#14679,#3004);
#2334=LINE('',#14682,#3005);
#2335=LINE('',#14684,#3006);
#2336=LINE('',#14685,#3007);
#2337=LINE('',#14688,#3008);
#2338=LINE('',#14690,#3009);
#2339=LINE('',#14691,#3010);
#2340=LINE('',#14694,#3011);
#2341=LINE('',#14696,#3012);
#2342=LINE('',#14697,#3013);
#2343=LINE('',#14700,#3014);
#2344=LINE('',#14702,#3015);
#2345=LINE('',#14703,#3016);
#2346=LINE('',#14706,#3017);
#2347=LINE('',#14708,#3018);
#2348=LINE('',#14709,#3019);
#2349=LINE('',#14711,#3020);
#2350=LINE('',#14712,#3021);
#2351=LINE('',#14719,#3022);
#2352=LINE('',#14721,#3023);
#2353=LINE('',#14723,#3024);
#2354=LINE('',#14724,#3025);
#2355=LINE('',#14727,#3026);
#2356=LINE('',#14729,#3027);
#2357=LINE('',#14730,#3028);
#2358=LINE('',#14733,#3029);
#2359=LINE('',#14735,#3030);
#2360=LINE('',#14736,#3031);
#2361=LINE('',#14739,#3032);
#2362=LINE('',#14741,#3033);
#2363=LINE('',#14742,#3034);
#2364=LINE('',#14745,#3035);
#2365=LINE('',#14747,#3036);
#2366=LINE('',#14748,#3037);
#2367=LINE('',#14751,#3038);
#2368=LINE('',#14753,#3039);
#2369=LINE('',#14754,#3040);
#2370=LINE('',#14757,#3041);
#2371=LINE('',#14759,#3042);
#2372=LINE('',#14760,#3043);
#2373=LINE('',#14762,#3044);
#2374=LINE('',#14763,#3045);
#2375=LINE('',#14773,#3046);
#2376=LINE('',#14775,#3047);
#2377=LINE('',#14777,#3048);
#2378=LINE('',#14778,#3049);
#2379=LINE('',#14781,#3050);
#2380=LINE('',#14783,#3051);
#2381=LINE('',#14784,#3052);
#2382=LINE('',#14787,#3053);
#2383=LINE('',#14789,#3054);
#2384=LINE('',#14790,#3055);
#2385=LINE('',#14793,#3056);
#2386=LINE('',#14795,#3057);
#2387=LINE('',#14796,#3058);
#2388=LINE('',#14799,#3059);
#2389=LINE('',#14801,#3060);
#2390=LINE('',#14802,#3061);
#2391=LINE('',#14804,#3062);
#2392=LINE('',#14805,#3063);
#2393=LINE('',#14817,#3064);
#2394=LINE('',#14821,#3065);
#2395=LINE('',#14825,#3066);
#2396=LINE('',#14832,#3067);
#2397=LINE('',#14834,#3068);
#2398=LINE('',#14842,#3069);
#2399=LINE('',#14846,#3070);
#2400=LINE('',#14850,#3071);
#2401=LINE('',#14857,#3072);
#2402=LINE('',#14861,#3073);
#2403=LINE('',#14865,#3074);
#2404=LINE('',#14870,#3075);
#2405=LINE('',#14872,#3076);
#2406=LINE('',#14874,#3077);
#2407=LINE('',#14875,#3078);
#2408=LINE('',#14878,#3079);
#2409=LINE('',#14880,#3080);
#2410=LINE('',#14881,#3081);
#2411=LINE('',#14884,#3082);
#2412=LINE('',#14886,#3083);
#2413=LINE('',#14887,#3084);
#2414=LINE('',#14890,#3085);
#2415=LINE('',#14892,#3086);
#2416=LINE('',#14893,#3087);
#2417=LINE('',#14896,#3088);
#2418=LINE('',#14898,#3089);
#2419=LINE('',#14899,#3090);
#2420=LINE('',#14901,#3091);
#2421=LINE('',#14902,#3092);
#2422=VECTOR('',#8231,0.21);
#2423=VECTOR('',#8240,0.21);
#2424=VECTOR('',#8249,0.165);
#2425=VECTOR('',#8258,0.164999999999999);
#2426=VECTOR('',#8267,0.275);
#2427=VECTOR('',#8272,1.);
#2428=VECTOR('',#8273,1.);
#2429=VECTOR('',#8274,1.);
#2430=VECTOR('',#8275,1.);
#2431=VECTOR('',#8278,1.);
#2432=VECTOR('',#8279,1.);
#2433=VECTOR('',#8280,1.);
#2434=VECTOR('',#8283,1.);
#2435=VECTOR('',#8284,1.);
#2436=VECTOR('',#8285,1.);
#2437=VECTOR('',#8288,1.);
#2438=VECTOR('',#8289,1.);
#2439=VECTOR('',#8298,1.);
#2440=VECTOR('',#8299,1.);
#2441=VECTOR('',#8300,1.);
#2442=VECTOR('',#8301,1.);
#2443=VECTOR('',#8304,1.);
#2444=VECTOR('',#8305,1.);
#2445=VECTOR('',#8306,1.);
#2446=VECTOR('',#8309,1.);
#2447=VECTOR('',#8310,1.);
#2448=VECTOR('',#8311,1.);
#2449=VECTOR('',#8314,1.);
#2450=VECTOR('',#8315,1.);
#2451=VECTOR('',#8324,1.);
#2452=VECTOR('',#8325,1.);
#2453=VECTOR('',#8326,1.);
#2454=VECTOR('',#8327,1.);
#2455=VECTOR('',#8330,1.);
#2456=VECTOR('',#8331,1.);
#2457=VECTOR('',#8332,1.);
#2458=VECTOR('',#8335,1.);
#2459=VECTOR('',#8336,1.);
#2460=VECTOR('',#8337,1.);
#2461=VECTOR('',#8340,1.);
#2462=VECTOR('',#8341,1.);
#2463=VECTOR('',#8352,0.275);
#2464=VECTOR('',#8357,1.);
#2465=VECTOR('',#8358,1.);
#2466=VECTOR('',#8359,1.);
#2467=VECTOR('',#8360,1.);
#2468=VECTOR('',#8363,1.);
#2469=VECTOR('',#8364,1.);
#2470=VECTOR('',#8365,1.);
#2471=VECTOR('',#8368,1.);
#2472=VECTOR('',#8369,1.);
#2473=VECTOR('',#8370,1.);
#2474=VECTOR('',#8373,1.);
#2475=VECTOR('',#8374,1.);
#2476=VECTOR('',#8385,0.210000000000001);
#2477=VECTOR('',#8392,0.210000000000001);
#2478=VECTOR('',#8399,0.164999999999999);
#2479=VECTOR('',#8406,0.164999999999999);
#2480=VECTOR('',#8413,0.164999999999999);
#2481=VECTOR('',#8420,0.164999999999999);
#2482=VECTOR('',#8427,0.274999999999999);
#2483=VECTOR('',#8434,0.275);
#2484=VECTOR('',#8439,1.);
#2485=VECTOR('',#8440,1.);
#2486=VECTOR('',#8441,1.);
#2487=VECTOR('',#8442,1.);
#2488=VECTOR('',#8445,1.);
#2489=VECTOR('',#8446,1.);
#2490=VECTOR('',#8447,1.);
#2491=VECTOR('',#8448,1.);
#2492=VECTOR('',#8451,1.);
#2493=VECTOR('',#8452,1.);
#2494=VECTOR('',#8455,1.);
#2495=VECTOR('',#8456,1.);
#2496=VECTOR('',#8457,1.);
#2497=VECTOR('',#8458,1.);
#2498=VECTOR('',#8459,1.);
#2499=VECTOR('',#8462,1.);
#2500=VECTOR('',#8463,1.);
#2501=VECTOR('',#8466,1.);
#2502=VECTOR('',#8467,1.);
#2503=VECTOR('',#8470,1.);
#2504=VECTOR('',#8471,1.);
#2505=VECTOR('',#8472,1.);
#2506=VECTOR('',#8475,1.);
#2507=VECTOR('',#8476,1.);
#2508=VECTOR('',#8487,0.275);
#2509=VECTOR('',#8492,1.);
#2510=VECTOR('',#8493,1.);
#2511=VECTOR('',#8494,1.);
#2512=VECTOR('',#8495,1.);
#2513=VECTOR('',#8498,1.);
#2514=VECTOR('',#8499,1.);
#2515=VECTOR('',#8500,1.);
#2516=VECTOR('',#8503,1.);
#2517=VECTOR('',#8504,1.);
#2518=VECTOR('',#8505,1.);
#2519=VECTOR('',#8508,1.);
#2520=VECTOR('',#8509,1.);
#2521=VECTOR('',#8520,0.274999999999999);
#2522=VECTOR('',#8525,1.);
#2523=VECTOR('',#8526,1.);
#2524=VECTOR('',#8527,1.);
#2525=VECTOR('',#8528,1.);
#2526=VECTOR('',#8531,1.);
#2527=VECTOR('',#8532,1.);
#2528=VECTOR('',#8533,1.);
#2529=VECTOR('',#8536,1.);
#2530=VECTOR('',#8537,1.);
#2531=VECTOR('',#8538,1.);
#2532=VECTOR('',#8541,1.);
#2533=VECTOR('',#8542,1.);
#2534=VECTOR('',#8553,0.225);
#2535=VECTOR('',#8560,0.225);
#2536=VECTOR('',#8567,1.1);
#2537=VECTOR('',#8574,1.5);
#2538=VECTOR('',#8585,2.2);
#2539=VECTOR('',#8598,1.1);
#2540=VECTOR('',#8605,1.3);
#2541=VECTOR('',#8618,0.225);
#2542=VECTOR('',#8625,0.225);
#2543=VECTOR('',#8632,1.01);
#2544=VECTOR('',#8643,1.09);
#2545=VECTOR('',#8652,0.605);
#2546=VECTOR('',#8657,2.2);
#2547=VECTOR('',#8680,0.300000000000001);
#2548=VECTOR('',#8683,0.199999999999999);
#2549=VECTOR('',#8690,0.199999999999999);
#2550=VECTOR('',#8701,0.164999999999999);
#2551=VECTOR('',#8708,0.4);
#2552=VECTOR('',#8731,0.3);
#2553=VECTOR('',#8734,0.2);
#2554=VECTOR('',#8741,0.2);
#2555=VECTOR('',#8752,0.165);
#2556=VECTOR('',#8759,0.4);
#2557=VECTOR('',#8786,1.);
#2558=VECTOR('',#8791,1.);
#2559=VECTOR('',#8794,1.);
#2560=VECTOR('',#8795,1.);
#2561=VECTOR('',#8796,1.);
#2562=VECTOR('',#8797,1.);
#2563=VECTOR('',#8800,1.);
#2564=VECTOR('',#8805,0.275);
#2565=VECTOR('',#8820,0.275);
#2566=VECTOR('',#8823,1.);
#2567=VECTOR('',#8824,1.);
#2568=VECTOR('',#8825,1.);
#2569=VECTOR('',#8828,1.);
#2570=VECTOR('',#8829,1.);
#2571=VECTOR('',#8844,1.);
#2572=VECTOR('',#8849,1.);
#2573=VECTOR('',#8852,1.);
#2574=VECTOR('',#8853,1.);
#2575=VECTOR('',#8854,1.);
#2576=VECTOR('',#8855,1.);
#2577=VECTOR('',#8858,1.);
#2578=VECTOR('',#8865,0.275);
#2579=VECTOR('',#8878,0.275);
#2580=VECTOR('',#8881,1.);
#2581=VECTOR('',#8882,1.);
#2582=VECTOR('',#8883,1.);
#2583=VECTOR('',#8886,1.);
#2584=VECTOR('',#8887,1.);
#2585=VECTOR('',#8896,1.);
#2586=VECTOR('',#8897,1.);
#2587=VECTOR('',#8898,1.);
#2588=VECTOR('',#8899,1.);
#2589=VECTOR('',#8902,1.);
#2590=VECTOR('',#8903,1.);
#2591=VECTOR('',#8904,1.);
#2592=VECTOR('',#8907,1.);
#2593=VECTOR('',#8908,1.);
#2594=VECTOR('',#8909,1.);
#2595=VECTOR('',#8912,1.);
#2596=VECTOR('',#8913,1.);
#2597=VECTOR('',#8914,1.);
#2598=VECTOR('',#8917,1.);
#2599=VECTOR('',#8918,1.);
#2600=VECTOR('',#8919,1.);
#2601=VECTOR('',#8922,1.);
#2602=VECTOR('',#8923,1.);
#2603=VECTOR('',#8924,1.);
#2604=VECTOR('',#8927,1.);
#2605=VECTOR('',#8928,1.);
#2606=VECTOR('',#8929,1.);
#2607=VECTOR('',#8932,1.);
#2608=VECTOR('',#8933,1.);
#2609=VECTOR('',#8934,1.);
#2610=VECTOR('',#8937,1.);
#2611=VECTOR('',#8938,1.);
#2612=VECTOR('',#8939,1.);
#2613=VECTOR('',#8942,1.);
#2614=VECTOR('',#8943,1.);
#2615=VECTOR('',#8944,1.);
#2616=VECTOR('',#8945,1.);
#2617=VECTOR('',#8948,1.);
#2618=VECTOR('',#8949,1.);
#2619=VECTOR('',#8950,1.);
#2620=VECTOR('',#8953,1.);
#2621=VECTOR('',#8954,1.);
#2622=VECTOR('',#8955,1.);
#2623=VECTOR('',#8958,1.);
#2624=VECTOR('',#8959,1.);
#2625=VECTOR('',#8960,1.);
#2626=VECTOR('',#8963,1.);
#2627=VECTOR('',#8964,1.);
#2628=VECTOR('',#8965,1.);
#2629=VECTOR('',#8968,1.);
#2630=VECTOR('',#8969,1.);
#2631=VECTOR('',#8970,1.);
#2632=VECTOR('',#8973,1.);
#2633=VECTOR('',#8974,1.);
#2634=VECTOR('',#8975,1.);
#2635=VECTOR('',#8978,1.);
#2636=VECTOR('',#8979,1.);
#2637=VECTOR('',#8980,1.);
#2638=VECTOR('',#8983,1.);
#2639=VECTOR('',#8984,1.);
#2640=VECTOR('',#8985,1.);
#2641=VECTOR('',#8988,1.);
#2642=VECTOR('',#8989,1.);
#2643=VECTOR('',#8990,1.);
#2644=VECTOR('',#8991,1.);
#2645=VECTOR('',#8994,1.);
#2646=VECTOR('',#8995,1.);
#2647=VECTOR('',#8996,1.);
#2648=VECTOR('',#8999,1.);
#2649=VECTOR('',#9000,1.);
#2650=VECTOR('',#9001,1.);
#2651=VECTOR('',#9004,1.);
#2652=VECTOR('',#9005,1.);
#2653=VECTOR('',#9006,1.);
#2654=VECTOR('',#9009,1.);
#2655=VECTOR('',#9010,1.);
#2656=VECTOR('',#9011,1.);
#2657=VECTOR('',#9014,1.);
#2658=VECTOR('',#9015,1.);
#2659=VECTOR('',#9016,1.);
#2660=VECTOR('',#9019,1.);
#2661=VECTOR('',#9020,1.);
#2662=VECTOR('',#9021,1.);
#2663=VECTOR('',#9024,1.);
#2664=VECTOR('',#9025,1.);
#2665=VECTOR('',#9026,1.);
#2666=VECTOR('',#9029,1.);
#2667=VECTOR('',#9030,1.);
#2668=VECTOR('',#9031,1.);
#2669=VECTOR('',#9034,1.);
#2670=VECTOR('',#9035,1.);
#2671=VECTOR('',#9036,1.);
#2672=VECTOR('',#9037,1.);
#2673=VECTOR('',#9040,1.);
#2674=VECTOR('',#9041,1.);
#2675=VECTOR('',#9042,1.);
#2676=VECTOR('',#9045,1.);
#2677=VECTOR('',#9046,1.);
#2678=VECTOR('',#9047,1.);
#2679=VECTOR('',#9050,1.);
#2680=VECTOR('',#9051,1.);
#2681=VECTOR('',#9052,1.);
#2682=VECTOR('',#9055,1.);
#2683=VECTOR('',#9056,1.);
#2684=VECTOR('',#9057,1.);
#2685=VECTOR('',#9060,1.);
#2686=VECTOR('',#9061,1.);
#2687=VECTOR('',#9062,1.);
#2688=VECTOR('',#9065,1.);
#2689=VECTOR('',#9066,1.);
#2690=VECTOR('',#9067,1.);
#2691=VECTOR('',#9070,1.);
#2692=VECTOR('',#9071,1.);
#2693=VECTOR('',#9072,1.);
#2694=VECTOR('',#9075,1.);
#2695=VECTOR('',#9076,1.);
#2696=VECTOR('',#9077,1.);
#2697=VECTOR('',#9082,0.21);
#2698=VECTOR('',#9087,1.);
#2699=VECTOR('',#9088,1.);
#2700=VECTOR('',#9089,1.);
#2701=VECTOR('',#9092,1.);
#2702=VECTOR('',#9093,1.);
#2703=VECTOR('',#9094,1.);
#2704=VECTOR('',#9097,1.);
#2705=VECTOR('',#9098,1.);
#2706=VECTOR('',#9101,1.);
#2707=VECTOR('',#9102,1.);
#2708=VECTOR('',#9103,1.);
#2709=VECTOR('',#9106,1.);
#2710=VECTOR('',#9107,1.);
#2711=VECTOR('',#9110,1.);
#2712=VECTOR('',#9111,1.);
#2713=VECTOR('',#9112,1.);
#2714=VECTOR('',#9115,1.);
#2715=VECTOR('',#9116,1.);
#2716=VECTOR('',#9119,1.);
#2717=VECTOR('',#9120,1.);
#2718=VECTOR('',#9131,0.375);
#2719=VECTOR('',#9142,0.375);
#2720=VECTOR('',#9153,0.375);
#2721=VECTOR('',#9164,0.375);
#2722=VECTOR('',#9175,0.225);
#2723=VECTOR('',#9180,0.225);
#2724=VECTOR('',#9185,0.225);
#2725=VECTOR('',#9190,0.225000000000001);
#2726=VECTOR('',#9193,1.);
#2727=VECTOR('',#9194,1.);
#2728=VECTOR('',#9195,1.);
#2729=VECTOR('',#9196,1.);
#2730=VECTOR('',#9199,1.);
#2731=VECTOR('',#9200,1.);
#2732=VECTOR('',#9201,1.);
#2733=VECTOR('',#9204,1.);
#2734=VECTOR('',#9205,1.);
#2735=VECTOR('',#9206,1.);
#2736=VECTOR('',#9209,1.);
#2737=VECTOR('',#9210,1.);
#2738=VECTOR('',#9211,1.);
#2739=VECTOR('',#9214,1.);
#2740=VECTOR('',#9215,1.);
#2741=VECTOR('',#9216,1.);
#2742=VECTOR('',#9219,1.);
#2743=VECTOR('',#9220,1.);
#2744=VECTOR('',#9221,1.);
#2745=VECTOR('',#9224,1.);
#2746=VECTOR('',#9225,1.);
#2747=VECTOR('',#9226,1.);
#2748=VECTOR('',#9229,1.);
#2749=VECTOR('',#9230,1.);
#2750=VECTOR('',#9231,1.);
#2751=VECTOR('',#9234,1.);
#2752=VECTOR('',#9235,1.);
#2753=VECTOR('',#9236,1.);
#2754=VECTOR('',#9239,1.);
#2755=VECTOR('',#9240,1.);
#2756=VECTOR('',#9241,1.);
#2757=VECTOR('',#9244,1.);
#2758=VECTOR('',#9245,1.);
#2759=VECTOR('',#9246,1.);
#2760=VECTOR('',#9249,1.);
#2761=VECTOR('',#9250,1.);
#2762=VECTOR('',#9259,1.);
#2763=VECTOR('',#9260,1.);
#2764=VECTOR('',#9261,1.);
#2765=VECTOR('',#9262,1.);
#2766=VECTOR('',#9265,1.);
#2767=VECTOR('',#9266,1.);
#2768=VECTOR('',#9267,1.);
#2769=VECTOR('',#9270,1.);
#2770=VECTOR('',#9271,1.);
#2771=VECTOR('',#9272,1.);
#2772=VECTOR('',#9275,1.);
#2773=VECTOR('',#9276,1.);
#2774=VECTOR('',#9277,1.);
#2775=VECTOR('',#9280,1.);
#2776=VECTOR('',#9281,1.);
#2777=VECTOR('',#9282,1.);
#2778=VECTOR('',#9285,1.);
#2779=VECTOR('',#9286,1.);
#2780=VECTOR('',#9299,0.25);
#2781=VECTOR('',#9312,0.4);
#2782=VECTOR('',#9317,0.425);
#2783=VECTOR('',#9322,0.41);
#2784=VECTOR('',#9331,0.26);
#2785=VECTOR('',#9334,0.25);
#2786=VECTOR('',#9345,0.4);
#2787=VECTOR('',#9350,0.425);
#2788=VECTOR('',#9355,0.41);
#2789=VECTOR('',#9364,0.26);
#2790=VECTOR('',#9369,0.25);
#2791=VECTOR('',#9374,0.225);
#2792=VECTOR('',#9379,1.);
#2793=VECTOR('',#9380,1.);
#2794=VECTOR('',#9381,1.);
#2795=VECTOR('',#9382,1.);
#2796=VECTOR('',#9385,1.);
#2797=VECTOR('',#9386,1.);
#2798=VECTOR('',#9387,1.);
#2799=VECTOR('',#9390,1.);
#2800=VECTOR('',#9391,1.);
#2801=VECTOR('',#9392,1.);
#2802=VECTOR('',#9395,1.);
#2803=VECTOR('',#9396,1.);
#2804=VECTOR('',#9397,1.);
#2805=VECTOR('',#9400,1.);
#2806=VECTOR('',#9401,1.);
#2807=VECTOR('',#9402,1.);
#2808=VECTOR('',#9405,1.);
#2809=VECTOR('',#9406,1.);
#2810=VECTOR('',#9415,1.);
#2811=VECTOR('',#9416,1.);
#2812=VECTOR('',#9417,1.);
#2813=VECTOR('',#9418,1.);
#2814=VECTOR('',#9421,1.);
#2815=VECTOR('',#9422,1.);
#2816=VECTOR('',#9423,1.);
#2817=VECTOR('',#9426,1.);
#2818=VECTOR('',#9427,1.);
#2819=VECTOR('',#9428,1.);
#2820=VECTOR('',#9433,1.);
#2821=VECTOR('',#9434,1.);
#2822=VECTOR('',#9435,1.);
#2823=VECTOR('',#9436,1.);
#2824=VECTOR('',#9437,1.);
#2825=VECTOR('',#9438,1.);
#2826=VECTOR('',#9439,1.);
#2827=VECTOR('',#9442,1.);
#2828=VECTOR('',#9443,1.);
#2829=VECTOR('',#9446,1.);
#2830=VECTOR('',#9447,1.);
#2831=VECTOR('',#9450,1.);
#2832=VECTOR('',#9451,1.);
#2833=VECTOR('',#9452,1.);
#2834=VECTOR('',#9453,1.);
#2835=VECTOR('',#9454,1.);
#2836=VECTOR('',#9457,1.);
#2837=VECTOR('',#9460,1.);
#2838=VECTOR('',#9463,1.);
#2839=VECTOR('',#9468,0.21);
#2840=VECTOR('',#9477,1.);
#2841=VECTOR('',#9480,1.);
#2842=VECTOR('',#9483,1.);
#2843=VECTOR('',#9492,0.275);
#2844=VECTOR('',#9497,0.265);
#2845=VECTOR('',#9506,0.5);
#2846=VECTOR('',#9519,0.225000000000001);
#2847=VECTOR('',#9524,1.);
#2848=VECTOR('',#9525,1.);
#2849=VECTOR('',#9526,1.);
#2850=VECTOR('',#9527,1.);
#2851=VECTOR('',#9530,1.);
#2852=VECTOR('',#9531,1.);
#2853=VECTOR('',#9532,1.);
#2854=VECTOR('',#9535,1.);
#2855=VECTOR('',#9536,1.);
#2856=VECTOR('',#9537,1.);
#2857=VECTOR('',#9540,1.);
#2858=VECTOR('',#9541,1.);
#2859=VECTOR('',#9542,1.);
#2860=VECTOR('',#9545,1.);
#2861=VECTOR('',#9546,1.);
#2862=VECTOR('',#9547,1.);
#2863=VECTOR('',#9548,1.);
#2864=VECTOR('',#9549,1.);
#2865=VECTOR('',#9554,0.525);
#2866=VECTOR('',#9561,0.45);
#2867=VECTOR('',#9568,0.449999999999999);
#2868=VECTOR('',#9573,1.);
#2869=VECTOR('',#9576,1.);
#2870=VECTOR('',#9581,1.);
#2871=VECTOR('',#9584,1.);
#2872=VECTOR('',#9585,1.);
#2873=VECTOR('',#9586,1.);
#2874=VECTOR('',#9589,1.);
#2875=VECTOR('',#9590,1.);
#2876=VECTOR('',#9601,0.274999999999999);
#2877=VECTOR('',#9606,1.);
#2878=VECTOR('',#9607,1.);
#2879=VECTOR('',#9608,1.);
#2880=VECTOR('',#9609,1.);
#2881=VECTOR('',#9610,1.);
#2882=VECTOR('',#9611,1.);
#2883=VECTOR('',#9612,1.);
#2884=VECTOR('',#9613,1.);
#2885=VECTOR('',#9616,0.274999999999999);
#2886=VECTOR('',#9627,0.274999999999999);
#2887=VECTOR('',#9632,0.274999999999999);
#2888=VECTOR('',#9637,1.);
#2889=VECTOR('',#9638,1.);
#2890=VECTOR('',#9639,1.);
#2891=VECTOR('',#9642,1.);
#2892=VECTOR('',#9643,1.);
#2893=VECTOR('',#9646,1.);
#2894=VECTOR('',#9647,1.);
#2895=VECTOR('',#9650,1.);
#2896=VECTOR('',#9651,1.);
#2897=VECTOR('',#9654,1.);
#2898=VECTOR('',#9657,1.);
#2899=VECTOR('',#9660,1.);
#2900=VECTOR('',#9661,1.);
#2901=VECTOR('',#9664,1.);
#2902=VECTOR('',#9665,1.);
#2903=VECTOR('',#9666,1.);
#2904=VECTOR('',#9669,1.);
#2905=VECTOR('',#9670,1.);
#2906=VECTOR('',#9681,0.425);
#2907=VECTOR('',#9688,1.09);
#2908=VECTOR('',#9701,0.5);
#2909=VECTOR('',#9710,0.5);
#2910=VECTOR('',#9725,1.);
#2911=VECTOR('',#9730,0.6);
#2912=VECTOR('',#9741,0.425);
#2913=VECTOR('',#9748,0.9);
#2914=VECTOR('',#9761,0.25);
#2915=VECTOR('',#9768,0.164999999999999);
#2916=VECTOR('',#9775,1.);
#2917=VECTOR('',#9776,1.);
#2918=VECTOR('',#9777,1.);
#2919=VECTOR('',#9778,1.);
#2920=VECTOR('',#9781,1.);
#2921=VECTOR('',#9782,1.);
#2922=VECTOR('',#9783,1.);
#2923=VECTOR('',#9786,1.);
#2924=VECTOR('',#9787,1.);
#2925=VECTOR('',#9788,1.);
#2926=VECTOR('',#9791,1.);
#2927=VECTOR('',#9792,1.);
#2928=VECTOR('',#9801,1.);
#2929=VECTOR('',#9802,1.);
#2930=VECTOR('',#9803,1.);
#2931=VECTOR('',#9804,1.);
#2932=VECTOR('',#9807,1.);
#2933=VECTOR('',#9808,1.);
#2934=VECTOR('',#9809,1.);
#2935=VECTOR('',#9812,1.);
#2936=VECTOR('',#9813,1.);
#2937=VECTOR('',#9814,1.);
#2938=VECTOR('',#9817,1.);
#2939=VECTOR('',#9818,1.);
#2940=VECTOR('',#9829,1.2);
#2941=VECTOR('',#9840,0.3);
#2942=VECTOR('',#9851,1.);
#2943=VECTOR('',#9856,1.);
#2944=VECTOR('',#9859,0.21);
#2945=VECTOR('',#9864,1.);
#2946=VECTOR('',#9867,1.);
#2947=VECTOR('',#9872,1.);
#2948=VECTOR('',#9875,0.21);
#2949=VECTOR('',#9880,1.);
#2950=VECTOR('',#9883,1.);
#2951=VECTOR('',#9888,1.);
#2952=VECTOR('',#9891,0.21);
#2953=VECTOR('',#9896,1.);
#2954=VECTOR('',#9899,1.);
#2955=VECTOR('',#9904,1.);
#2956=VECTOR('',#9907,0.21);
#2957=VECTOR('',#9912,1.);
#2958=VECTOR('',#9915,1.);
#2959=VECTOR('',#9916,1.);
#2960=VECTOR('',#9917,1.);
#2961=VECTOR('',#9918,1.);
#2962=VECTOR('',#9919,1.);
#2963=VECTOR('',#9920,1.);
#2964=VECTOR('',#9923,1.);
#2965=VECTOR('',#9924,1.);
#2966=VECTOR('',#9925,1.);
#2967=VECTOR('',#9926,1.);
#2968=VECTOR('',#9927,1.);
#2969=VECTOR('',#9928,1.);
#2970=VECTOR('',#9931,1.);
#2971=VECTOR('',#9932,1.);
#2972=VECTOR('',#9933,1.);
#2973=VECTOR('',#9934,1.);
#2974=VECTOR('',#9935,1.);
#2975=VECTOR('',#9936,1.);
#2976=VECTOR('',#9937,1.);
#2977=VECTOR('',#9938,1.);
#2978=VECTOR('',#9939,1.);
#2979=VECTOR('',#9940,1.);
#2980=VECTOR('',#9943,1.);
#2981=VECTOR('',#9944,1.);
#2982=VECTOR('',#9947,1.);
#2983=VECTOR('',#9948,1.);
#2984=VECTOR('',#9951,1.);
#2985=VECTOR('',#9952,1.);
#2986=VECTOR('',#9955,1.);
#2987=VECTOR('',#9956,1.);
#2988=VECTOR('',#9959,1.);
#2989=VECTOR('',#9962,1.);
#2990=VECTOR('',#9963,1.);
#2991=VECTOR('',#9966,1.);
#2992=VECTOR('',#9967,1.);
#2993=VECTOR('',#9970,1.);
#2994=VECTOR('',#9971,1.);
#2995=VECTOR('',#9974,1.);
#2996=VECTOR('',#9975,1.);
#2997=VECTOR('',#9978,1.);
#2998=VECTOR('',#9985,1.);
#2999=VECTOR('',#9986,1.);
#3000=VECTOR('',#9987,1.);
#3001=VECTOR('',#9988,1.);
#3002=VECTOR('',#9991,1.);
#3003=VECTOR('',#9992,1.);
#3004=VECTOR('',#9993,1.);
#3005=VECTOR('',#9996,1.);
#3006=VECTOR('',#9997,1.);
#3007=VECTOR('',#9998,1.);
#3008=VECTOR('',#10001,1.);
#3009=VECTOR('',#10002,1.);
#3010=VECTOR('',#10003,1.);
#3011=VECTOR('',#10006,1.);
#3012=VECTOR('',#10007,1.);
#3013=VECTOR('',#10008,1.);
#3014=VECTOR('',#10011,1.);
#3015=VECTOR('',#10012,1.);
#3016=VECTOR('',#10013,1.);
#3017=VECTOR('',#10016,1.);
#3018=VECTOR('',#10017,1.);
#3019=VECTOR('',#10018,1.);
#3020=VECTOR('',#10021,1.);
#3021=VECTOR('',#10022,1.);
#3022=VECTOR('',#10031,1.);
#3023=VECTOR('',#10032,1.);
#3024=VECTOR('',#10033,1.);
#3025=VECTOR('',#10034,1.);
#3026=VECTOR('',#10037,1.);
#3027=VECTOR('',#10038,1.);
#3028=VECTOR('',#10039,1.);
#3029=VECTOR('',#10042,1.);
#3030=VECTOR('',#10043,1.);
#3031=VECTOR('',#10044,1.);
#3032=VECTOR('',#10047,1.);
#3033=VECTOR('',#10048,1.);
#3034=VECTOR('',#10049,1.);
#3035=VECTOR('',#10052,1.);
#3036=VECTOR('',#10053,1.);
#3037=VECTOR('',#10054,1.);
#3038=VECTOR('',#10057,1.);
#3039=VECTOR('',#10058,1.);
#3040=VECTOR('',#10059,1.);
#3041=VECTOR('',#10062,1.);
#3042=VECTOR('',#10063,1.);
#3043=VECTOR('',#10064,1.);
#3044=VECTOR('',#10067,1.);
#3045=VECTOR('',#10068,1.);
#3046=VECTOR('',#10083,1.);
#3047=VECTOR('',#10084,1.);
#3048=VECTOR('',#10085,1.);
#3049=VECTOR('',#10086,1.);
#3050=VECTOR('',#10089,1.);
#3051=VECTOR('',#10090,1.);
#3052=VECTOR('',#10091,1.);
#3053=VECTOR('',#10094,1.);
#3054=VECTOR('',#10095,1.);
#3055=VECTOR('',#10096,1.);
#3056=VECTOR('',#10099,1.);
#3057=VECTOR('',#10100,1.);
#3058=VECTOR('',#10101,1.);
#3059=VECTOR('',#10104,1.);
#3060=VECTOR('',#10105,1.);
#3061=VECTOR('',#10106,1.);
#3062=VECTOR('',#10109,1.);
#3063=VECTOR('',#10110,1.);
#3064=VECTOR('',#10127,0.4);
#3065=VECTOR('',#10132,0.425);
#3066=VECTOR('',#10137,0.41);
#3067=VECTOR('',#10146,0.26);
#3068=VECTOR('',#10149,0.25);
#3069=VECTOR('',#10160,0.325);
#3070=VECTOR('',#10165,0.35);
#3071=VECTOR('',#10170,0.335);
#3072=VECTOR('',#10179,0.21);
#3073=VECTOR('',#10184,0.2);
#3074=VECTOR('',#10189,0.18);
#3075=VECTOR('',#10194,1.);
#3076=VECTOR('',#10195,1.);
#3077=VECTOR('',#10196,1.);
#3078=VECTOR('',#10197,1.);
#3079=VECTOR('',#10200,1.);
#3080=VECTOR('',#10201,1.);
#3081=VECTOR('',#10202,1.);
#3082=VECTOR('',#10205,1.);
#3083=VECTOR('',#10206,1.);
#3084=VECTOR('',#10207,1.);
#3085=VECTOR('',#10210,1.);
#3086=VECTOR('',#10211,1.);
#3087=VECTOR('',#10212,1.);
#3088=VECTOR('',#10215,1.);
#3089=VECTOR('',#10216,1.);
#3090=VECTOR('',#10217,1.);
#3091=VECTOR('',#10220,1.);
#3092=VECTOR('',#10221,1.);
#3093=CIRCLE('',#7502,0.21);
#3094=CIRCLE('',#7503,0.21);
#3095=CIRCLE('',#7506,0.21);
#3096=CIRCLE('',#7507,0.21);
#3097=CIRCLE('',#7510,0.165);
#3098=CIRCLE('',#7511,0.165);
#3099=CIRCLE('',#7514,0.164999999999999);
#3100=CIRCLE('',#7515,0.164999999999999);
#3101=CIRCLE('',#7518,0.275);
#3102=CIRCLE('',#7519,0.275);
#3103=CIRCLE('',#7542,0.275);
#3104=CIRCLE('',#7543,0.275);
#3105=CIRCLE('',#7552,0.210000000000001);
#3106=CIRCLE('',#7553,0.210000000000001);
#3107=CIRCLE('',#7555,0.210000000000001);
#3108=CIRCLE('',#7556,0.210000000000001);
#3109=CIRCLE('',#7558,0.164999999999999);
#3110=CIRCLE('',#7559,0.164999999999999);
#3111=CIRCLE('',#7561,0.164999999999999);
#3112=CIRCLE('',#7562,0.164999999999999);
#3113=CIRCLE('',#7564,0.164999999999999);
#3114=CIRCLE('',#7565,0.164999999999999);
#3115=CIRCLE('',#7567,0.164999999999999);
#3116=CIRCLE('',#7568,0.164999999999999);
#3117=CIRCLE('',#7570,0.274999999999999);
#3118=CIRCLE('',#7571,0.274999999999999);
#3119=CIRCLE('',#7573,0.275);
#3120=CIRCLE('',#7574,0.275);
#3121=CIRCLE('',#7587,0.275);
#3122=CIRCLE('',#7588,0.275);
#3123=CIRCLE('',#7597,0.274999999999999);
#3124=CIRCLE('',#7598,0.274999999999999);
#3125=CIRCLE('',#7607,0.225);
#3126=CIRCLE('',#7608,0.225);
#3127=CIRCLE('',#7610,0.225);
#3128=CIRCLE('',#7611,0.225);
#3129=CIRCLE('',#7613,1.1);
#3130=CIRCLE('',#7614,1.1);
#3131=CIRCLE('',#7616,1.5);
#3132=CIRCLE('',#7617,1.5);
#3133=CIRCLE('',#7620,2.2);
#3134=CIRCLE('',#7622,2.2);
#3135=CIRCLE('',#7627,1.1);
#3136=CIRCLE('',#7628,1.1);
#3137=CIRCLE('',#7630,1.3);
#3138=CIRCLE('',#7631,1.3);
#3139=CIRCLE('',#7636,0.225);
#3140=CIRCLE('',#7637,0.225);
#3141=CIRCLE('',#7639,0.225);
#3142=CIRCLE('',#7640,0.225);
#3143=CIRCLE('',#7642,1.01);
#3144=CIRCLE('',#7643,1.01);
#3145=CIRCLE('',#7645,0.605);
#3146=CIRCLE('',#7647,1.09);
#3147=CIRCLE('',#7648,1.09);
#3148=CIRCLE('',#7650,0.605);
#3149=CIRCLE('',#7653,2.2);
#3150=CIRCLE('',#7654,2.2);
#3151=CIRCLE('',#7659,0.300000000000001);
#3152=CIRCLE('',#7660,0.199999999999999);
#3153=CIRCLE('',#7662,0.300000000000001);
#3154=CIRCLE('',#7663,0.199999999999999);
#3155=CIRCLE('',#7666,0.199999999999999);
#3156=CIRCLE('',#7668,0.199999999999999);
#3157=CIRCLE('',#7673,0.164999999999999);
#3158=CIRCLE('',#7674,0.164999999999999);
#3159=CIRCLE('',#7676,0.4);
#3160=CIRCLE('',#7677,0.4);
#3161=CIRCLE('',#7682,0.3);
#3162=CIRCLE('',#7683,0.2);
#3163=CIRCLE('',#7685,0.3);
#3164=CIRCLE('',#7686,0.2);
#3165=CIRCLE('',#7689,0.2);
#3166=CIRCLE('',#7691,0.2);
#3167=CIRCLE('',#7696,0.165);
#3168=CIRCLE('',#7697,0.165);
#3169=CIRCLE('',#7699,0.4);
#3170=CIRCLE('',#7700,0.4);
#3171=CIRCLE('',#7704,0.05);
#3172=CIRCLE('',#7705,0.05);
#3173=CIRCLE('',#7711,0.5);
#3174=CIRCLE('',#7713,0.275);
#3175=CIRCLE('',#7714,0.275);
#3176=CIRCLE('',#7719,0.275);
#3177=CIRCLE('',#7721,0.5);
#3178=CIRCLE('',#7722,0.275);
#3179=CIRCLE('',#7725,0.275);
#3180=CIRCLE('',#7733,0.5);
#3181=CIRCLE('',#7735,0.275);
#3182=CIRCLE('',#7736,0.275);
#3183=CIRCLE('',#7741,0.275);
#3184=CIRCLE('',#7743,0.5);
#3185=CIRCLE('',#7744,0.275);
#3186=CIRCLE('',#7747,0.275);
#3187=CIRCLE('',#7790,0.21);
#3188=CIRCLE('',#7791,0.21);
#3189=CIRCLE('',#7804,0.375);
#3190=CIRCLE('',#7805,0.375);
#3191=CIRCLE('',#7807,0.225);
#3192=CIRCLE('',#7809,0.375);
#3193=CIRCLE('',#7810,0.375);
#3194=CIRCLE('',#7812,0.225);
#3195=CIRCLE('',#7814,0.375);
#3196=CIRCLE('',#7815,0.375);
#3197=CIRCLE('',#7817,0.225);
#3198=CIRCLE('',#7819,0.375);
#3199=CIRCLE('',#7820,0.375);
#3200=CIRCLE('',#7822,0.225000000000001);
#3201=CIRCLE('',#7824,0.225);
#3202=CIRCLE('',#7826,0.225);
#3203=CIRCLE('',#7828,0.225);
#3204=CIRCLE('',#7830,0.225000000000001);
#3205=CIRCLE('',#7855,0.25);
#3206=CIRCLE('',#7856,0.24505);
#3207=CIRCLE('',#7858,0.25);
#3208=CIRCLE('',#7861,0.375);
#3209=CIRCLE('',#7863,0.425);
#3210=CIRCLE('',#7865,0.425);
#3211=CIRCLE('',#7867,0.395);
#3212=CIRCLE('',#7869,0.27);
#3213=CIRCLE('',#7871,0.24505);
#3214=CIRCLE('',#7875,0.375);
#3215=CIRCLE('',#7877,0.425);
#3216=CIRCLE('',#7879,0.425);
#3217=CIRCLE('',#7881,0.395);
#3218=CIRCLE('',#7883,0.27);
#3219=CIRCLE('',#7885,0.24505);
#3220=CIRCLE('',#7887,0.24505);
#3221=CIRCLE('',#7889,0.2);
#3222=CIRCLE('',#7903,0.2117);
#3223=CIRCLE('',#7912,0.2117);
#3224=CIRCLE('',#7913,0.2117);
#3225=CIRCLE('',#7915,0.2117);
#3226=CIRCLE('',#7922,0.285);
#3227=CIRCLE('',#7923,0.265);
#3228=CIRCLE('',#7925,0.265);
#3229=CIRCLE('',#7927,0.5);
#3230=CIRCLE('',#7929,0.5);
#3231=CIRCLE('',#7934,0.225000000000001);
#3232=CIRCLE('',#7935,0.225000000000001);
#3233=CIRCLE('',#7942,0.525);
#3234=CIRCLE('',#7943,0.525);
#3235=CIRCLE('',#7945,0.45);
#3236=CIRCLE('',#7946,0.45);
#3237=CIRCLE('',#7948,0.449999999999999);
#3238=CIRCLE('',#7949,0.449999999999999);
#3239=CIRCLE('',#7951,0.5);
#3240=CIRCLE('',#7952,0.5);
#3241=CIRCLE('',#7955,0.5);
#3242=CIRCLE('',#7956,0.274999999999999);
#3243=CIRCLE('',#7957,0.274999999999999);
#3244=CIRCLE('',#7958,0.274999999999999);
#3245=CIRCLE('',#7959,0.274999999999999);
#3246=CIRCLE('',#7961,0.274999999999999);
#3247=CIRCLE('',#7964,0.274999999999999);
#3248=CIRCLE('',#7966,0.5);
#3249=CIRCLE('',#7969,0.274999999999999);
#3250=CIRCLE('',#7971,0.274999999999999);
#3251=CIRCLE('',#7985,0.425);
#3252=CIRCLE('',#7986,0.425);
#3253=CIRCLE('',#7988,1.09);
#3254=CIRCLE('',#7989,1.09);
#3255=CIRCLE('',#7994,0.5);
#3256=CIRCLE('',#7995,0.5);
#3257=CIRCLE('',#7998,0.5);
#3258=CIRCLE('',#7999,0.5);
#3259=CIRCLE('',#8002,1.);
#3260=CIRCLE('',#8003,0.6);
#3261=CIRCLE('',#8005,1.);
#3262=CIRCLE('',#8008,0.6);
#3263=CIRCLE('',#8012,0.425);
#3264=CIRCLE('',#8013,0.425);
#3265=CIRCLE('',#8015,0.9);
#3266=CIRCLE('',#8016,0.9);
#3267=CIRCLE('',#8021,0.25);
#3268=CIRCLE('',#8022,0.25);
#3269=CIRCLE('',#8024,0.164999999999999);
#3270=CIRCLE('',#8025,0.164999999999999);
#3271=CIRCLE('',#8042,1.2);
#3272=CIRCLE('',#8043,1.2);
#3273=CIRCLE('',#8046,0.3);
#3274=CIRCLE('',#8048,0.3);
#3275=CIRCLE('',#8053,0.21);
#3276=CIRCLE('',#8055,0.21);
#3277=CIRCLE('',#8056,0.21);
#3278=CIRCLE('',#8057,0.21);
#3279=CIRCLE('',#8059,0.21);
#3280=CIRCLE('',#8061,0.21);
#3281=CIRCLE('',#8062,0.21);
#3282=CIRCLE('',#8063,0.21);
#3283=CIRCLE('',#8065,0.21);
#3284=CIRCLE('',#8067,0.21);
#3285=CIRCLE('',#8068,0.21);
#3286=CIRCLE('',#8069,0.21);
#3287=CIRCLE('',#8071,0.21);
#3288=CIRCLE('',#8073,0.21);
#3289=CIRCLE('',#8074,0.21);
#3290=CIRCLE('',#8075,0.21);
#3291=CIRCLE('',#8125,0.24505);
#3292=CIRCLE('',#8127,0.375);
#3293=CIRCLE('',#8129,0.425);
#3294=CIRCLE('',#8131,0.425);
#3295=CIRCLE('',#8133,0.395);
#3296=CIRCLE('',#8135,0.27);
#3297=CIRCLE('',#8137,0.24505);
#3298=CIRCLE('',#8141,0.3);
#3299=CIRCLE('',#8143,0.35);
#3300=CIRCLE('',#8145,0.35);
#3301=CIRCLE('',#8147,0.32);
#3302=CIRCLE('',#8149,0.22);
#3303=CIRCLE('',#8151,0.1954);
#3304=CIRCLE('',#8153,0.1954);
#3305=CIRCLE('',#8155,0.16);
#3306=VERTEX_POINT('',#10342);
#3307=VERTEX_POINT('',#10344);
#3308=VERTEX_POINT('',#10349);
#3309=VERTEX_POINT('',#10351);
#3310=VERTEX_POINT('',#10356);
#3311=VERTEX_POINT('',#10358);
#3312=VERTEX_POINT('',#10363);
#3313=VERTEX_POINT('',#10365);
#3314=VERTEX_POINT('',#10370);
#3315=VERTEX_POINT('',#10372);
#3316=VERTEX_POINT('',#10376);
#3317=VERTEX_POINT('',#10377);
#3318=VERTEX_POINT('',#10379);
#3319=VERTEX_POINT('',#10381);
#3320=VERTEX_POINT('',#10385);
#3321=VERTEX_POINT('',#10387);
#3322=VERTEX_POINT('',#10391);
#3323=VERTEX_POINT('',#10393);
#3324=VERTEX_POINT('',#10403);
#3325=VERTEX_POINT('',#10404);
#3326=VERTEX_POINT('',#10406);
#3327=VERTEX_POINT('',#10408);
#3328=VERTEX_POINT('',#10412);
#3329=VERTEX_POINT('',#10414);
#3330=VERTEX_POINT('',#10418);
#3331=VERTEX_POINT('',#10420);
#3332=VERTEX_POINT('',#10430);
#3333=VERTEX_POINT('',#10431);
#3334=VERTEX_POINT('',#10433);
#3335=VERTEX_POINT('',#10435);
#3336=VERTEX_POINT('',#10439);
#3337=VERTEX_POINT('',#10441);
#3338=VERTEX_POINT('',#10445);
#3339=VERTEX_POINT('',#10447);
#3340=VERTEX_POINT('',#10457);
#3341=VERTEX_POINT('',#10459);
#3342=VERTEX_POINT('',#10463);
#3343=VERTEX_POINT('',#10464);
#3344=VERTEX_POINT('',#10466);
#3345=VERTEX_POINT('',#10468);
#3346=VERTEX_POINT('',#10472);
#3347=VERTEX_POINT('',#10474);
#3348=VERTEX_POINT('',#10478);
#3349=VERTEX_POINT('',#10480);
#3350=VERTEX_POINT('',#10490);
#3351=VERTEX_POINT('',#10492);
#3352=VERTEX_POINT('',#10496);
#3353=VERTEX_POINT('',#10498);
#3354=VERTEX_POINT('',#10502);
#3355=VERTEX_POINT('',#10504);
#3356=VERTEX_POINT('',#10508);
#3357=VERTEX_POINT('',#10510);
#3358=VERTEX_POINT('',#10514);
#3359=VERTEX_POINT('',#10516);
#3360=VERTEX_POINT('',#10520);
#3361=VERTEX_POINT('',#10522);
#3362=VERTEX_POINT('',#10526);
#3363=VERTEX_POINT('',#10528);
#3364=VERTEX_POINT('',#10532);
#3365=VERTEX_POINT('',#10534);
#3366=VERTEX_POINT('',#10538);
#3367=VERTEX_POINT('',#10539);
#3368=VERTEX_POINT('',#10541);
#3369=VERTEX_POINT('',#10543);
#3370=VERTEX_POINT('',#10547);
#3371=VERTEX_POINT('',#10548);
#3372=VERTEX_POINT('',#10550);
#3373=VERTEX_POINT('',#10552);
#3374=VERTEX_POINT('',#10559);
#3375=VERTEX_POINT('',#10561);
#3376=VERTEX_POINT('',#10563);
#3377=VERTEX_POINT('',#10565);
#3378=VERTEX_POINT('',#10569);
#3379=VERTEX_POINT('',#10573);
#3380=VERTEX_POINT('',#10577);
#3381=VERTEX_POINT('',#10579);
#3382=VERTEX_POINT('',#10589);
#3383=VERTEX_POINT('',#10591);
#3384=VERTEX_POINT('',#10595);
#3385=VERTEX_POINT('',#10596);
#3386=VERTEX_POINT('',#10598);
#3387=VERTEX_POINT('',#10600);
#3388=VERTEX_POINT('',#10604);
#3389=VERTEX_POINT('',#10606);
#3390=VERTEX_POINT('',#10610);
#3391=VERTEX_POINT('',#10612);
#3392=VERTEX_POINT('',#10622);
#3393=VERTEX_POINT('',#10624);
#3394=VERTEX_POINT('',#10628);
#3395=VERTEX_POINT('',#10629);
#3396=VERTEX_POINT('',#10631);
#3397=VERTEX_POINT('',#10633);
#3398=VERTEX_POINT('',#10637);
#3399=VERTEX_POINT('',#10639);
#3400=VERTEX_POINT('',#10643);
#3401=VERTEX_POINT('',#10645);
#3402=VERTEX_POINT('',#10655);
#3403=VERTEX_POINT('',#10657);
#3404=VERTEX_POINT('',#10661);
#3405=VERTEX_POINT('',#10663);
#3406=VERTEX_POINT('',#10667);
#3407=VERTEX_POINT('',#10669);
#3408=VERTEX_POINT('',#10673);
#3409=VERTEX_POINT('',#10675);
#3410=VERTEX_POINT('',#10680);
#3411=VERTEX_POINT('',#10683);
#3412=VERTEX_POINT('',#10690);
#3413=VERTEX_POINT('',#10692);
#3414=VERTEX_POINT('',#10696);
#3415=VERTEX_POINT('',#10698);
#3416=VERTEX_POINT('',#10705);
#3417=VERTEX_POINT('',#10707);
#3418=VERTEX_POINT('',#10711);
#3419=VERTEX_POINT('',#10713);
#3420=VERTEX_POINT('',#10717);
#3421=VERTEX_POINT('',#10719);
#3422=VERTEX_POINT('',#10723);
#3423=VERTEX_POINT('',#10726);
#3424=VERTEX_POINT('',#10728);
#3425=VERTEX_POINT('',#10732);
#3426=VERTEX_POINT('',#10737);
#3427=VERTEX_POINT('',#10739);
#3428=VERTEX_POINT('',#10746);
#3429=VERTEX_POINT('',#10748);
#3430=VERTEX_POINT('',#10751);
#3431=VERTEX_POINT('',#10753);
#3432=VERTEX_POINT('',#10758);
#3433=VERTEX_POINT('',#10762);
#3434=VERTEX_POINT('',#10769);
#3435=VERTEX_POINT('',#10771);
#3436=VERTEX_POINT('',#10775);
#3437=VERTEX_POINT('',#10777);
#3438=VERTEX_POINT('',#10784);
#3439=VERTEX_POINT('',#10786);
#3440=VERTEX_POINT('',#10789);
#3441=VERTEX_POINT('',#10791);
#3442=VERTEX_POINT('',#10796);
#3443=VERTEX_POINT('',#10800);
#3444=VERTEX_POINT('',#10807);
#3445=VERTEX_POINT('',#10809);
#3446=VERTEX_POINT('',#10813);
#3447=VERTEX_POINT('',#10815);
#3448=VERTEX_POINT('',#13221);
#3449=VERTEX_POINT('',#13223);
#3450=VERTEX_POINT('',#13469);
#3451=VERTEX_POINT('',#13470);
#3452=VERTEX_POINT('',#13474);
#3453=VERTEX_POINT('',#13476);
#3454=VERTEX_POINT('',#13478);
#3455=VERTEX_POINT('',#13482);
#3456=VERTEX_POINT('',#13483);
#3457=VERTEX_POINT('',#13485);
#3458=VERTEX_POINT('',#13487);
#3459=VERTEX_POINT('',#13490);
#3460=VERTEX_POINT('',#13491);
#3461=VERTEX_POINT('',#13496);
#3462=VERTEX_POINT('',#13501);
#3463=VERTEX_POINT('',#13505);
#3464=VERTEX_POINT('',#13509);
#3465=VERTEX_POINT('',#13511);
#3466=VERTEX_POINT('',#13521);
#3467=VERTEX_POINT('',#13522);
#3468=VERTEX_POINT('',#13526);
#3469=VERTEX_POINT('',#13528);
#3470=VERTEX_POINT('',#13530);
#3471=VERTEX_POINT('',#13534);
#3472=VERTEX_POINT('',#13535);
#3473=VERTEX_POINT('',#13537);
#3474=VERTEX_POINT('',#13539);
#3475=VERTEX_POINT('',#13542);
#3476=VERTEX_POINT('',#13543);
#3477=VERTEX_POINT('',#13548);
#3478=VERTEX_POINT('',#13553);
#3479=VERTEX_POINT('',#13557);
#3480=VERTEX_POINT('',#13561);
#3481=VERTEX_POINT('',#13563);
#3482=VERTEX_POINT('',#13573);
#3483=VERTEX_POINT('',#13574);
#3484=VERTEX_POINT('',#13576);
#3485=VERTEX_POINT('',#13578);
#3486=VERTEX_POINT('',#13582);
#3487=VERTEX_POINT('',#13584);
#3488=VERTEX_POINT('',#13588);
#3489=VERTEX_POINT('',#13590);
#3490=VERTEX_POINT('',#13594);
#3491=VERTEX_POINT('',#13596);
#3492=VERTEX_POINT('',#13600);
#3493=VERTEX_POINT('',#13602);
#3494=VERTEX_POINT('',#13606);
#3495=VERTEX_POINT('',#13608);
#3496=VERTEX_POINT('',#13612);
#3497=VERTEX_POINT('',#13614);
#3498=VERTEX_POINT('',#13618);
#3499=VERTEX_POINT('',#13620);
#3500=VERTEX_POINT('',#13624);
#3501=VERTEX_POINT('',#13626);
#3502=VERTEX_POINT('',#13630);
#3503=VERTEX_POINT('',#13631);
#3504=VERTEX_POINT('',#13633);
#3505=VERTEX_POINT('',#13635);
#3506=VERTEX_POINT('',#13639);
#3507=VERTEX_POINT('',#13641);
#3508=VERTEX_POINT('',#13645);
#3509=VERTEX_POINT('',#13647);
#3510=VERTEX_POINT('',#13651);
#3511=VERTEX_POINT('',#13653);
#3512=VERTEX_POINT('',#13657);
#3513=VERTEX_POINT('',#13659);
#3514=VERTEX_POINT('',#13663);
#3515=VERTEX_POINT('',#13665);
#3516=VERTEX_POINT('',#13669);
#3517=VERTEX_POINT('',#13671);
#3518=VERTEX_POINT('',#13675);
#3519=VERTEX_POINT('',#13677);
#3520=VERTEX_POINT('',#13681);
#3521=VERTEX_POINT('',#13683);
#3522=VERTEX_POINT('',#13687);
#3523=VERTEX_POINT('',#13688);
#3524=VERTEX_POINT('',#13690);
#3525=VERTEX_POINT('',#13692);
#3526=VERTEX_POINT('',#13696);
#3527=VERTEX_POINT('',#13698);
#3528=VERTEX_POINT('',#13702);
#3529=VERTEX_POINT('',#13704);
#3530=VERTEX_POINT('',#13708);
#3531=VERTEX_POINT('',#13710);
#3532=VERTEX_POINT('',#13714);
#3533=VERTEX_POINT('',#13716);
#3534=VERTEX_POINT('',#13720);
#3535=VERTEX_POINT('',#13722);
#3536=VERTEX_POINT('',#13726);
#3537=VERTEX_POINT('',#13728);
#3538=VERTEX_POINT('',#13732);
#3539=VERTEX_POINT('',#13734);
#3540=VERTEX_POINT('',#13738);
#3541=VERTEX_POINT('',#13740);
#3542=VERTEX_POINT('',#13744);
#3543=VERTEX_POINT('',#13745);
#3544=VERTEX_POINT('',#13747);
#3545=VERTEX_POINT('',#13749);
#3546=VERTEX_POINT('',#13753);
#3547=VERTEX_POINT('',#13755);
#3548=VERTEX_POINT('',#13759);
#3549=VERTEX_POINT('',#13761);
#3550=VERTEX_POINT('',#13765);
#3551=VERTEX_POINT('',#13767);
#3552=VERTEX_POINT('',#13771);
#3553=VERTEX_POINT('',#13773);
#3554=VERTEX_POINT('',#13777);
#3555=VERTEX_POINT('',#13779);
#3556=VERTEX_POINT('',#13783);
#3557=VERTEX_POINT('',#13785);
#3558=VERTEX_POINT('',#13789);
#3559=VERTEX_POINT('',#13791);
#3560=VERTEX_POINT('',#13795);
#3561=VERTEX_POINT('',#13797);
#3562=VERTEX_POINT('',#13801);
#3563=VERTEX_POINT('',#13803);
#3564=VERTEX_POINT('',#13807);
#3565=VERTEX_POINT('',#13809);
#3566=VERTEX_POINT('',#13813);
#3567=VERTEX_POINT('',#13815);
#3568=VERTEX_POINT('',#13822);
#3569=VERTEX_POINT('',#13824);
#3570=VERTEX_POINT('',#13831);
#3571=VERTEX_POINT('',#13833);
#3572=VERTEX_POINT('',#13846);
#3573=VERTEX_POINT('',#13848);
#3574=VERTEX_POINT('',#13852);
#3575=VERTEX_POINT('',#13855);
#3576=VERTEX_POINT('',#13857);
#3577=VERTEX_POINT('',#13861);
#3578=VERTEX_POINT('',#13864);
#3579=VERTEX_POINT('',#13866);
#3580=VERTEX_POINT('',#13870);
#3581=VERTEX_POINT('',#13873);
#3582=VERTEX_POINT('',#13875);
#3583=VERTEX_POINT('',#13879);
#3584=VERTEX_POINT('',#13882);
#3585=VERTEX_POINT('',#13886);
#3586=VERTEX_POINT('',#13890);
#3587=VERTEX_POINT('',#13894);
#3588=VERTEX_POINT('',#13898);
#3589=VERTEX_POINT('',#13899);
#3590=VERTEX_POINT('',#13901);
#3591=VERTEX_POINT('',#13903);
#3592=VERTEX_POINT('',#13907);
#3593=VERTEX_POINT('',#13909);
#3594=VERTEX_POINT('',#13913);
#3595=VERTEX_POINT('',#13915);
#3596=VERTEX_POINT('',#13919);
#3597=VERTEX_POINT('',#13921);
#3598=VERTEX_POINT('',#13925);
#3599=VERTEX_POINT('',#13927);
#3600=VERTEX_POINT('',#13931);
#3601=VERTEX_POINT('',#13933);
#3602=VERTEX_POINT('',#13937);
#3603=VERTEX_POINT('',#13939);
#3604=VERTEX_POINT('',#13943);
#3605=VERTEX_POINT('',#13945);
#3606=VERTEX_POINT('',#13949);
#3607=VERTEX_POINT('',#13951);
#3608=VERTEX_POINT('',#13955);
#3609=VERTEX_POINT('',#13957);
#3610=VERTEX_POINT('',#13961);
#3611=VERTEX_POINT('',#13963);
#3612=VERTEX_POINT('',#13973);
#3613=VERTEX_POINT('',#13974);
#3614=VERTEX_POINT('',#13976);
#3615=VERTEX_POINT('',#13978);
#3616=VERTEX_POINT('',#13982);
#3617=VERTEX_POINT('',#13984);
#3618=VERTEX_POINT('',#13988);
#3619=VERTEX_POINT('',#13990);
#3620=VERTEX_POINT('',#13994);
#3621=VERTEX_POINT('',#13996);
#3622=VERTEX_POINT('',#14000);
#3623=VERTEX_POINT('',#14002);
#3624=VERTEX_POINT('',#14011);
#3625=VERTEX_POINT('',#14013);
#3626=VERTEX_POINT('',#14016);
#3627=VERTEX_POINT('',#14021);
#3628=VERTEX_POINT('',#14024);
#3629=VERTEX_POINT('',#14028);
#3630=VERTEX_POINT('',#14032);
#3631=VERTEX_POINT('',#14036);
#3632=VERTEX_POINT('',#14039);
#3633=VERTEX_POINT('',#14046);
#3634=VERTEX_POINT('',#14049);
#3635=VERTEX_POINT('',#14053);
#3636=VERTEX_POINT('',#14057);
#3637=VERTEX_POINT('',#14061);
#3638=VERTEX_POINT('',#14064);
#3639=VERTEX_POINT('',#14068);
#3640=VERTEX_POINT('',#14072);
#3641=VERTEX_POINT('',#14077);
#3642=VERTEX_POINT('',#14078);
#3643=VERTEX_POINT('',#14080);
#3644=VERTEX_POINT('',#14082);
#3645=VERTEX_POINT('',#14086);
#3646=VERTEX_POINT('',#14088);
#3647=VERTEX_POINT('',#14092);
#3648=VERTEX_POINT('',#14094);
#3649=VERTEX_POINT('',#14098);
#3650=VERTEX_POINT('',#14100);
#3651=VERTEX_POINT('',#14104);
#3652=VERTEX_POINT('',#14106);
#3653=VERTEX_POINT('',#14116);
#3654=VERTEX_POINT('',#14117);
#3655=VERTEX_POINT('',#14119);
#3656=VERTEX_POINT('',#14121);
#3657=VERTEX_POINT('',#14125);
#3658=VERTEX_POINT('',#14127);
#3659=VERTEX_POINT('',#14131);
#3660=VERTEX_POINT('',#14133);
#3661=VERTEX_POINT('',#14136);
#3662=VERTEX_POINT('',#14139);
#3663=VERTEX_POINT('',#14141);
#3664=VERTEX_POINT('',#14143);
#3665=VERTEX_POINT('',#14145);
#3666=VERTEX_POINT('',#14147);
#3667=VERTEX_POINT('',#14149);
#3668=VERTEX_POINT('',#14153);
#3669=VERTEX_POINT('',#14157);
#3670=VERTEX_POINT('',#14161);
#3671=VERTEX_POINT('',#14163);
#3672=VERTEX_POINT('',#14165);
#3673=VERTEX_POINT('',#14167);
#3674=VERTEX_POINT('',#14173);
#3675=VERTEX_POINT('',#14175);
#3676=VERTEX_POINT('',#14179);
#3677=VERTEX_POINT('',#14182);
#3678=VERTEX_POINT('',#14184);
#3679=VERTEX_POINT('',#14196);
#3680=VERTEX_POINT('',#14198);
#3681=VERTEX_POINT('',#14202);
#3682=VERTEX_POINT('',#14206);
#3683=VERTEX_POINT('',#14209);
#3684=VERTEX_POINT('',#14216);
#3685=VERTEX_POINT('',#14218);
#3686=VERTEX_POINT('',#14222);
#3687=VERTEX_POINT('',#14223);
#3688=VERTEX_POINT('',#14225);
#3689=VERTEX_POINT('',#14227);
#3690=VERTEX_POINT('',#14231);
#3691=VERTEX_POINT('',#14233);
#3692=VERTEX_POINT('',#14237);
#3693=VERTEX_POINT('',#14238);
#3694=VERTEX_POINT('',#14243);
#3695=VERTEX_POINT('',#14245);
#3696=VERTEX_POINT('',#14249);
#3697=VERTEX_POINT('',#14251);
#3698=VERTEX_POINT('',#14253);
#3699=VERTEX_POINT('',#14255);
#3700=VERTEX_POINT('',#14259);
#3701=VERTEX_POINT('',#14261);
#3702=VERTEX_POINT('',#14265);
#3703=VERTEX_POINT('',#14267);
#3704=VERTEX_POINT('',#14271);
#3705=VERTEX_POINT('',#14273);
#3706=VERTEX_POINT('',#14277);
#3707=VERTEX_POINT('',#14278);
#3708=VERTEX_POINT('',#14280);
#3709=VERTEX_POINT('',#14282);
#3710=VERTEX_POINT('',#14288);
#3711=VERTEX_POINT('',#14290);
#3712=VERTEX_POINT('',#14292);
#3713=VERTEX_POINT('',#14294);
#3714=VERTEX_POINT('',#14298);
#3715=VERTEX_POINT('',#14300);
#3716=VERTEX_POINT('',#14302);
#3717=VERTEX_POINT('',#14304);
#3718=VERTEX_POINT('',#14307);
#3719=VERTEX_POINT('',#14311);
#3720=VERTEX_POINT('',#14313);
#3721=VERTEX_POINT('',#14316);
#3722=VERTEX_POINT('',#14318);
#3723=VERTEX_POINT('',#14320);
#3724=VERTEX_POINT('',#14322);
#3725=VERTEX_POINT('',#14326);
#3726=VERTEX_POINT('',#14333);
#3727=VERTEX_POINT('',#14337);
#3728=VERTEX_POINT('',#14341);
#3729=VERTEX_POINT('',#14343);
#3730=VERTEX_POINT('',#14347);
#3731=VERTEX_POINT('',#14351);
#3732=VERTEX_POINT('',#14355);
#3733=VERTEX_POINT('',#14363);
#3734=VERTEX_POINT('',#14367);
#3735=VERTEX_POINT('',#14369);
#3736=VERTEX_POINT('',#14379);
#3737=VERTEX_POINT('',#14381);
#3738=VERTEX_POINT('',#14385);
#3739=VERTEX_POINT('',#14387);
#3740=VERTEX_POINT('',#14394);
#3741=VERTEX_POINT('',#14396);
#3742=VERTEX_POINT('',#14401);
#3743=VERTEX_POINT('',#14403);
#3744=VERTEX_POINT('',#14408);
#3745=VERTEX_POINT('',#14410);
#3746=VERTEX_POINT('',#14413);
#3747=VERTEX_POINT('',#14418);
#3748=VERTEX_POINT('',#14424);
#3749=VERTEX_POINT('',#14426);
#3750=VERTEX_POINT('',#14430);
#3751=VERTEX_POINT('',#14432);
#3752=VERTEX_POINT('',#14439);
#3753=VERTEX_POINT('',#14441);
#3754=VERTEX_POINT('',#14445);
#3755=VERTEX_POINT('',#14447);
#3756=VERTEX_POINT('',#14452);
#3757=VERTEX_POINT('',#14453);
#3758=VERTEX_POINT('',#14455);
#3759=VERTEX_POINT('',#14457);
#3760=VERTEX_POINT('',#14461);
#3761=VERTEX_POINT('',#14463);
#3762=VERTEX_POINT('',#14467);
#3763=VERTEX_POINT('',#14469);
#3764=VERTEX_POINT('',#14479);
#3765=VERTEX_POINT('',#14480);
#3766=VERTEX_POINT('',#14482);
#3767=VERTEX_POINT('',#14484);
#3768=VERTEX_POINT('',#14488);
#3769=VERTEX_POINT('',#14490);
#3770=VERTEX_POINT('',#14494);
#3771=VERTEX_POINT('',#14496);
#3772=VERTEX_POINT('',#14506);
#3773=VERTEX_POINT('',#14508);
#3774=VERTEX_POINT('',#14513);
#3775=VERTEX_POINT('',#14516);
#3776=VERTEX_POINT('',#14523);
#3777=VERTEX_POINT('',#14524);
#3778=VERTEX_POINT('',#14528);
#3779=VERTEX_POINT('',#14530);
#3780=VERTEX_POINT('',#14532);
#3781=VERTEX_POINT('',#14535);
#3782=VERTEX_POINT('',#14539);
#3783=VERTEX_POINT('',#14540);
#3784=VERTEX_POINT('',#14544);
#3785=VERTEX_POINT('',#14546);
#3786=VERTEX_POINT('',#14548);
#3787=VERTEX_POINT('',#14551);
#3788=VERTEX_POINT('',#14555);
#3789=VERTEX_POINT('',#14556);
#3790=VERTEX_POINT('',#14560);
#3791=VERTEX_POINT('',#14562);
#3792=VERTEX_POINT('',#14564);
#3793=VERTEX_POINT('',#14567);
#3794=VERTEX_POINT('',#14571);
#3795=VERTEX_POINT('',#14572);
#3796=VERTEX_POINT('',#14576);
#3797=VERTEX_POINT('',#14578);
#3798=VERTEX_POINT('',#14580);
#3799=VERTEX_POINT('',#14583);
#3800=VERTEX_POINT('',#14588);
#3801=VERTEX_POINT('',#14590);
#3802=VERTEX_POINT('',#14592);
#3803=VERTEX_POINT('',#14594);
#3804=VERTEX_POINT('',#14599);
#3805=VERTEX_POINT('',#14601);
#3806=VERTEX_POINT('',#14603);
#3807=VERTEX_POINT('',#14605);
#3808=VERTEX_POINT('',#14609);
#3809=VERTEX_POINT('',#14611);
#3810=VERTEX_POINT('',#14613);
#3811=VERTEX_POINT('',#14615);
#3812=VERTEX_POINT('',#14618);
#3813=VERTEX_POINT('',#14620);
#3814=VERTEX_POINT('',#14622);
#3815=VERTEX_POINT('',#14624);
#3816=VERTEX_POINT('',#14628);
#3817=VERTEX_POINT('',#14632);
#3818=VERTEX_POINT('',#14636);
#3819=VERTEX_POINT('',#14640);
#3820=VERTEX_POINT('',#14646);
#3821=VERTEX_POINT('',#14650);
#3822=VERTEX_POINT('',#14654);
#3823=VERTEX_POINT('',#14658);
#3824=VERTEX_POINT('',#14666);
#3825=VERTEX_POINT('',#14667);
#3826=VERTEX_POINT('',#14669);
#3827=VERTEX_POINT('',#14671);
#3828=VERTEX_POINT('',#14675);
#3829=VERTEX_POINT('',#14677);
#3830=VERTEX_POINT('',#14681);
#3831=VERTEX_POINT('',#14683);
#3832=VERTEX_POINT('',#14687);
#3833=VERTEX_POINT('',#14689);
#3834=VERTEX_POINT('',#14693);
#3835=VERTEX_POINT('',#14695);
#3836=VERTEX_POINT('',#14699);
#3837=VERTEX_POINT('',#14701);
#3838=VERTEX_POINT('',#14705);
#3839=VERTEX_POINT('',#14707);
#3840=VERTEX_POINT('',#14717);
#3841=VERTEX_POINT('',#14718);
#3842=VERTEX_POINT('',#14720);
#3843=VERTEX_POINT('',#14722);
#3844=VERTEX_POINT('',#14726);
#3845=VERTEX_POINT('',#14728);
#3846=VERTEX_POINT('',#14732);
#3847=VERTEX_POINT('',#14734);
#3848=VERTEX_POINT('',#14738);
#3849=VERTEX_POINT('',#14740);
#3850=VERTEX_POINT('',#14744);
#3851=VERTEX_POINT('',#14746);
#3852=VERTEX_POINT('',#14750);
#3853=VERTEX_POINT('',#14752);
#3854=VERTEX_POINT('',#14756);
#3855=VERTEX_POINT('',#14758);
#3856=VERTEX_POINT('',#14771);
#3857=VERTEX_POINT('',#14772);
#3858=VERTEX_POINT('',#14774);
#3859=VERTEX_POINT('',#14776);
#3860=VERTEX_POINT('',#14780);
#3861=VERTEX_POINT('',#14782);
#3862=VERTEX_POINT('',#14786);
#3863=VERTEX_POINT('',#14788);
#3864=VERTEX_POINT('',#14792);
#3865=VERTEX_POINT('',#14794);
#3866=VERTEX_POINT('',#14798);
#3867=VERTEX_POINT('',#14800);
#3868=VERTEX_POINT('',#14809);
#3869=VERTEX_POINT('',#14812);
#3870=VERTEX_POINT('',#14815);
#3871=VERTEX_POINT('',#14819);
#3872=VERTEX_POINT('',#14823);
#3873=VERTEX_POINT('',#14827);
#3874=VERTEX_POINT('',#14830);
#3875=VERTEX_POINT('',#14837);
#3876=VERTEX_POINT('',#14840);
#3877=VERTEX_POINT('',#14844);
#3878=VERTEX_POINT('',#14848);
#3879=VERTEX_POINT('',#14852);
#3880=VERTEX_POINT('',#14855);
#3881=VERTEX_POINT('',#14859);
#3882=VERTEX_POINT('',#14863);
#3883=VERTEX_POINT('',#14868);
#3884=VERTEX_POINT('',#14869);
#3885=VERTEX_POINT('',#14871);
#3886=VERTEX_POINT('',#14873);
#3887=VERTEX_POINT('',#14877);
#3888=VERTEX_POINT('',#14879);
#3889=VERTEX_POINT('',#14883);
#3890=VERTEX_POINT('',#14885);
#3891=VERTEX_POINT('',#14889);
#3892=VERTEX_POINT('',#14891);
#3893=VERTEX_POINT('',#14895);
#3894=VERTEX_POINT('',#14897);
#3895=EDGE_CURVE('',#3306,#3306,#3093,.T.);
#3896=EDGE_CURVE('',#3306,#3307,#1751,.T.);
#3897=EDGE_CURVE('',#3307,#3307,#3094,.T.);
#3898=EDGE_CURVE('',#3308,#3308,#3095,.T.);
#3899=EDGE_CURVE('',#3308,#3309,#1752,.T.);
#3900=EDGE_CURVE('',#3309,#3309,#3096,.T.);
#3901=EDGE_CURVE('',#3310,#3310,#3097,.T.);
#3902=EDGE_CURVE('',#3310,#3311,#1753,.T.);
#3903=EDGE_CURVE('',#3311,#3311,#3098,.T.);
#3904=EDGE_CURVE('',#3312,#3312,#3099,.T.);
#3905=EDGE_CURVE('',#3312,#3313,#1754,.T.);
#3906=EDGE_CURVE('',#3313,#3313,#3100,.T.);
#3907=EDGE_CURVE('',#3314,#3314,#3101,.T.);
#3908=EDGE_CURVE('',#3314,#3315,#1755,.T.);
#3909=EDGE_CURVE('',#3315,#3315,#3102,.T.);
#3910=EDGE_CURVE('',#3316,#3317,#1756,.T.);
#3911=EDGE_CURVE('',#3317,#3318,#1757,.T.);
#3912=EDGE_CURVE('',#3319,#3318,#1758,.T.);
#3913=EDGE_CURVE('',#3316,#3319,#1759,.T.);
#3914=EDGE_CURVE('',#3320,#3316,#1760,.T.);
#3915=EDGE_CURVE('',#3321,#3319,#1761,.T.);
#3916=EDGE_CURVE('',#3320,#3321,#1762,.T.);
#3917=EDGE_CURVE('',#3322,#3320,#1763,.T.);
#3918=EDGE_CURVE('',#3323,#3321,#1764,.T.);
#3919=EDGE_CURVE('',#3322,#3323,#1765,.T.);
#3920=EDGE_CURVE('',#3317,#3322,#1766,.T.);
#3921=EDGE_CURVE('',#3318,#3323,#1767,.T.);
#3922=EDGE_CURVE('',#3324,#3325,#1768,.T.);
#3923=EDGE_CURVE('',#3325,#3326,#1769,.T.);
#3924=EDGE_CURVE('',#3327,#3326,#1770,.T.);
#3925=EDGE_CURVE('',#3324,#3327,#1771,.T.);
#3926=EDGE_CURVE('',#3328,#3324,#1772,.T.);
#3927=EDGE_CURVE('',#3329,#3327,#1773,.T.);
#3928=EDGE_CURVE('',#3328,#3329,#1774,.T.);
#3929=EDGE_CURVE('',#3330,#3328,#1775,.T.);
#3930=EDGE_CURVE('',#3331,#3329,#1776,.T.);
#3931=EDGE_CURVE('',#3330,#3331,#1777,.T.);
#3932=EDGE_CURVE('',#3325,#3330,#1778,.T.);
#3933=EDGE_CURVE('',#3326,#3331,#1779,.T.);
#3934=EDGE_CURVE('',#3332,#3333,#1780,.T.);
#3935=EDGE_CURVE('',#3333,#3334,#1781,.T.);
#3936=EDGE_CURVE('',#3335,#3334,#1782,.T.);
#3937=EDGE_CURVE('',#3332,#3335,#1783,.T.);
#3938=EDGE_CURVE('',#3336,#3332,#1784,.T.);
#3939=EDGE_CURVE('',#3337,#3335,#1785,.T.);
#3940=EDGE_CURVE('',#3336,#3337,#1786,.T.);
#3941=EDGE_CURVE('',#3338,#3336,#1787,.T.);
#3942=EDGE_CURVE('',#3339,#3337,#1788,.T.);
#3943=EDGE_CURVE('',#3338,#3339,#1789,.T.);
#3944=EDGE_CURVE('',#3333,#3338,#1790,.T.);
#3945=EDGE_CURVE('',#3334,#3339,#1791,.T.);
#3946=EDGE_CURVE('',#3340,#3340,#3103,.T.);
#3947=EDGE_CURVE('',#3340,#3341,#1792,.T.);
#3948=EDGE_CURVE('',#3341,#3341,#3104,.T.);
#3949=EDGE_CURVE('',#3342,#3343,#1793,.T.);
#3950=EDGE_CURVE('',#3343,#3344,#1794,.T.);
#3951=EDGE_CURVE('',#3345,#3344,#1795,.T.);
#3952=EDGE_CURVE('',#3342,#3345,#1796,.T.);
#3953=EDGE_CURVE('',#3346,#3342,#1797,.T.);
#3954=EDGE_CURVE('',#3347,#3345,#1798,.T.);
#3955=EDGE_CURVE('',#3346,#3347,#1799,.T.);
#3956=EDGE_CURVE('',#3348,#3346,#1800,.T.);
#3957=EDGE_CURVE('',#3349,#3347,#1801,.T.);
#3958=EDGE_CURVE('',#3348,#3349,#1802,.T.);
#3959=EDGE_CURVE('',#3343,#3348,#1803,.T.);
#3960=EDGE_CURVE('',#3344,#3349,#1804,.T.);
#3961=EDGE_CURVE('',#3350,#3350,#3105,.T.);
#3962=EDGE_CURVE('',#3350,#3351,#1805,.T.);
#3963=EDGE_CURVE('',#3351,#3351,#3106,.T.);
#3964=EDGE_CURVE('',#3352,#3352,#3107,.T.);
#3965=EDGE_CURVE('',#3352,#3353,#1806,.T.);
#3966=EDGE_CURVE('',#3353,#3353,#3108,.T.);
#3967=EDGE_CURVE('',#3354,#3354,#3109,.T.);
#3968=EDGE_CURVE('',#3354,#3355,#1807,.T.);
#3969=EDGE_CURVE('',#3355,#3355,#3110,.T.);
#3970=EDGE_CURVE('',#3356,#3356,#3111,.T.);
#3971=EDGE_CURVE('',#3356,#3357,#1808,.T.);
#3972=EDGE_CURVE('',#3357,#3357,#3112,.T.);
#3973=EDGE_CURVE('',#3358,#3358,#3113,.T.);
#3974=EDGE_CURVE('',#3358,#3359,#1809,.T.);
#3975=EDGE_CURVE('',#3359,#3359,#3114,.T.);
#3976=EDGE_CURVE('',#3360,#3360,#3115,.T.);
#3977=EDGE_CURVE('',#3360,#3361,#1810,.T.);
#3978=EDGE_CURVE('',#3361,#3361,#3116,.T.);
#3979=EDGE_CURVE('',#3362,#3362,#3117,.T.);
#3980=EDGE_CURVE('',#3362,#3363,#1811,.T.);
#3981=EDGE_CURVE('',#3363,#3363,#3118,.T.);
#3982=EDGE_CURVE('',#3364,#3364,#3119,.T.);
#3983=EDGE_CURVE('',#3364,#3365,#1812,.T.);
#3984=EDGE_CURVE('',#3365,#3365,#3120,.T.);
#3985=EDGE_CURVE('',#3366,#3367,#1813,.T.);
#3986=EDGE_CURVE('',#3368,#3366,#1814,.T.);
#3987=EDGE_CURVE('',#3369,#3368,#1815,.T.);
#3988=EDGE_CURVE('',#3367,#3369,#1816,.T.);
#3989=EDGE_CURVE('',#3370,#3371,#1817,.T.);
#3990=EDGE_CURVE('',#3372,#3370,#1818,.T.);
#3991=EDGE_CURVE('',#3373,#3372,#1819,.T.);
#3992=EDGE_CURVE('',#3373,#3371,#1820,.T.);
#3993=EDGE_CURVE('',#3371,#3366,#1821,.T.);
#3994=EDGE_CURVE('',#3368,#3373,#1822,.T.);
#3995=EDGE_CURVE('',#3374,#3372,#1823,.T.);
#3996=EDGE_CURVE('',#3374,#3375,#1824,.T.);
#3997=EDGE_CURVE('',#3375,#3376,#1825,.T.);
#3998=EDGE_CURVE('',#3377,#3376,#1826,.T.);
#3999=EDGE_CURVE('',#3369,#3377,#1827,.T.);
#4000=EDGE_CURVE('',#3378,#3370,#1828,.T.);
#4001=EDGE_CURVE('',#3378,#3374,#1829,.T.);
#4002=EDGE_CURVE('',#3379,#3377,#1830,.T.);
#4003=EDGE_CURVE('',#3367,#3379,#1831,.T.);
#4004=EDGE_CURVE('',#3380,#3379,#1832,.T.);
#4005=EDGE_CURVE('',#3381,#3380,#1833,.T.);
#4006=EDGE_CURVE('',#3381,#3378,#1834,.T.);
#4007=EDGE_CURVE('',#3375,#3381,#1835,.T.);
#4008=EDGE_CURVE('',#3376,#3380,#1836,.T.);
#4009=EDGE_CURVE('',#3382,#3382,#3121,.T.);
#4010=EDGE_CURVE('',#3382,#3383,#1837,.T.);
#4011=EDGE_CURVE('',#3383,#3383,#3122,.T.);
#4012=EDGE_CURVE('',#3384,#3385,#1838,.T.);
#4013=EDGE_CURVE('',#3385,#3386,#1839,.T.);
#4014=EDGE_CURVE('',#3387,#3386,#1840,.T.);
#4015=EDGE_CURVE('',#3384,#3387,#1841,.T.);
#4016=EDGE_CURVE('',#3388,#3384,#1842,.T.);
#4017=EDGE_CURVE('',#3389,#3387,#1843,.T.);
#4018=EDGE_CURVE('',#3388,#3389,#1844,.T.);
#4019=EDGE_CURVE('',#3390,#3388,#1845,.T.);
#4020=EDGE_CURVE('',#3391,#3389,#1846,.T.);
#4021=EDGE_CURVE('',#3390,#3391,#1847,.T.);
#4022=EDGE_CURVE('',#3385,#3390,#1848,.T.);
#4023=EDGE_CURVE('',#3386,#3391,#1849,.T.);
#4024=EDGE_CURVE('',#3392,#3392,#3123,.T.);
#4025=EDGE_CURVE('',#3392,#3393,#1850,.T.);
#4026=EDGE_CURVE('',#3393,#3393,#3124,.T.);
#4027=EDGE_CURVE('',#3394,#3395,#1851,.T.);
#4028=EDGE_CURVE('',#3395,#3396,#1852,.T.);
#4029=EDGE_CURVE('',#3397,#3396,#1853,.T.);
#4030=EDGE_CURVE('',#3394,#3397,#1854,.T.);
#4031=EDGE_CURVE('',#3398,#3394,#1855,.T.);
#4032=EDGE_CURVE('',#3399,#3397,#1856,.T.);
#4033=EDGE_CURVE('',#3398,#3399,#1857,.T.);
#4034=EDGE_CURVE('',#3400,#3398,#1858,.T.);
#4035=EDGE_CURVE('',#3401,#3399,#1859,.T.);
#4036=EDGE_CURVE('',#3400,#3401,#1860,.T.);
#4037=EDGE_CURVE('',#3395,#3400,#1861,.T.);
#4038=EDGE_CURVE('',#3396,#3401,#1862,.T.);
#4039=EDGE_CURVE('',#3402,#3402,#3125,.T.);
#4040=EDGE_CURVE('',#3402,#3403,#1863,.T.);
#4041=EDGE_CURVE('',#3403,#3403,#3126,.T.);
#4042=EDGE_CURVE('',#3404,#3404,#3127,.T.);
#4043=EDGE_CURVE('',#3404,#3405,#1864,.T.);
#4044=EDGE_CURVE('',#3405,#3405,#3128,.T.);
#4045=EDGE_CURVE('',#3406,#3406,#3129,.T.);
#4046=EDGE_CURVE('',#3406,#3407,#1865,.T.);
#4047=EDGE_CURVE('',#3407,#3407,#3130,.T.);
#4048=EDGE_CURVE('',#3408,#3408,#3131,.T.);
#4049=EDGE_CURVE('',#3408,#3409,#1866,.T.);
#4050=EDGE_CURVE('',#3409,#3409,#3132,.T.);
#4051=EDGE_CURVE('',#3410,#3410,#3133,.T.);
#4052=EDGE_CURVE('',#3410,#3411,#1867,.T.);
#4053=EDGE_CURVE('',#3411,#3411,#3134,.T.);
#4054=EDGE_CURVE('',#3412,#3412,#3135,.T.);
#4055=EDGE_CURVE('',#3412,#3413,#1868,.T.);
#4056=EDGE_CURVE('',#3413,#3413,#3136,.T.);
#4057=EDGE_CURVE('',#3414,#3414,#3137,.T.);
#4058=EDGE_CURVE('',#3414,#3415,#1869,.T.);
#4059=EDGE_CURVE('',#3415,#3415,#3138,.T.);
#4060=EDGE_CURVE('',#3416,#3416,#3139,.T.);
#4061=EDGE_CURVE('',#3416,#3417,#1870,.T.);
#4062=EDGE_CURVE('',#3417,#3417,#3140,.T.);
#4063=EDGE_CURVE('',#3418,#3418,#3141,.T.);
#4064=EDGE_CURVE('',#3418,#3419,#1871,.T.);
#4065=EDGE_CURVE('',#3419,#3419,#3142,.T.);
#4066=EDGE_CURVE('',#3420,#3420,#3143,.T.);
#4067=EDGE_CURVE('',#3420,#3421,#1872,.T.);
#4068=EDGE_CURVE('',#3421,#3421,#3144,.T.);
#4069=EDGE_CURVE('',#3422,#3422,#3145,.T.);
#4070=EDGE_CURVE('',#3423,#3423,#3146,.T.);
#4071=EDGE_CURVE('',#3423,#3424,#1873,.T.);
#4072=EDGE_CURVE('',#3424,#3424,#3147,.T.);
#4073=EDGE_CURVE('',#3425,#3425,#3148,.T.);
#4074=EDGE_CURVE('',#3422,#3425,#1874,.T.);
#4075=EDGE_CURVE('',#3426,#3426,#3149,.T.);
#4076=EDGE_CURVE('',#3426,#3427,#1875,.T.);
#4077=EDGE_CURVE('',#3427,#3427,#3150,.T.);
#4078=EDGE_CURVE('',#3428,#3428,#3151,.T.);
#4079=EDGE_CURVE('',#3429,#3429,#3152,.T.);
#4080=EDGE_CURVE('',#3430,#3430,#3153,.T.);
#4081=EDGE_CURVE('',#3431,#3431,#3154,.T.);
#4082=EDGE_CURVE('',#3428,#3430,#1876,.T.);
#4083=EDGE_CURVE('',#3431,#3432,#1877,.T.);
#4084=EDGE_CURVE('',#3432,#3432,#3155,.T.);
#4085=EDGE_CURVE('',#3433,#3433,#3156,.T.);
#4086=EDGE_CURVE('',#3433,#3429,#1878,.T.);
#4087=EDGE_CURVE('',#3434,#3434,#3157,.T.);
#4088=EDGE_CURVE('',#3434,#3435,#1879,.T.);
#4089=EDGE_CURVE('',#3435,#3435,#3158,.T.);
#4090=EDGE_CURVE('',#3436,#3436,#3159,.T.);
#4091=EDGE_CURVE('',#3436,#3437,#1880,.T.);
#4092=EDGE_CURVE('',#3437,#3437,#3160,.T.);
#4093=EDGE_CURVE('',#3438,#3438,#3161,.T.);
#4094=EDGE_CURVE('',#3439,#3439,#3162,.T.);
#4095=EDGE_CURVE('',#3440,#3440,#3163,.T.);
#4096=EDGE_CURVE('',#3441,#3441,#3164,.T.);
#4097=EDGE_CURVE('',#3438,#3440,#1881,.T.);
#4098=EDGE_CURVE('',#3441,#3442,#1882,.T.);
#4099=EDGE_CURVE('',#3442,#3442,#3165,.T.);
#4100=EDGE_CURVE('',#3443,#3443,#3166,.T.);
#4101=EDGE_CURVE('',#3443,#3439,#1883,.T.);
#4102=EDGE_CURVE('',#3444,#3444,#3167,.T.);
#4103=EDGE_CURVE('',#3444,#3445,#1884,.T.);
#4104=EDGE_CURVE('',#3445,#3445,#3168,.T.);
#4105=EDGE_CURVE('',#3446,#3446,#3169,.T.);
#4106=EDGE_CURVE('',#3446,#3447,#1885,.T.);
#4107=EDGE_CURVE('',#3447,#3447,#3170,.T.);
#4108=EDGE_CURVE('',#3448,#3448,#3171,.T.);
#4109=EDGE_CURVE('',#3448,#3449,#278,.T.);
#4110=EDGE_CURVE('',#3449,#3449,#3172,.T.);
#4111=EDGE_CURVE('',#3450,#3451,#270,.T.);
#4112=EDGE_CURVE('',#3450,#3451,#3173,.T.);
#4113=EDGE_CURVE('',#3452,#3450,#1886,.T.);
#4114=EDGE_CURVE('',#3453,#3452,#3174,.T.);
#4115=EDGE_CURVE('',#3454,#3453,#3175,.T.);
#4116=EDGE_CURVE('',#3451,#3454,#1887,.T.);
#4117=EDGE_CURVE('',#3455,#3456,#1888,.T.);
#4118=EDGE_CURVE('',#3455,#3457,#1889,.T.);
#4119=EDGE_CURVE('',#3458,#3457,#1890,.T.);
#4120=EDGE_CURVE('',#3456,#3458,#1891,.T.);
#4121=EDGE_CURVE('',#3459,#3460,#271,.T.);
#4122=EDGE_CURVE('',#3460,#3459,#1892,.T.);
#4123=EDGE_CURVE('',#3454,#3452,#272,.T.);
#4124=EDGE_CURVE('',#3453,#3461,#1893,.T.);
#4125=EDGE_CURVE('',#3461,#3461,#3176,.T.);
#4126=EDGE_CURVE('',#3460,#3459,#3177,.T.);
#4127=EDGE_CURVE('',#3462,#3462,#3178,.T.);
#4128=EDGE_CURVE('',#3463,#3463,#3179,.T.);
#4129=EDGE_CURVE('',#3463,#3462,#1894,.T.);
#4130=EDGE_CURVE('',#3456,#3464,#1895,.T.);
#4131=EDGE_CURVE('',#3465,#3458,#1896,.T.);
#4132=EDGE_CURVE('',#3464,#3465,#1897,.T.);
#4133=EDGE_CURVE('',#3464,#3455,#1898,.T.);
#4134=EDGE_CURVE('',#3457,#3465,#1899,.T.);
#4135=EDGE_CURVE('',#3466,#3467,#273,.T.);
#4136=EDGE_CURVE('',#3467,#3466,#3180,.T.);
#4137=EDGE_CURVE('',#3468,#3466,#1900,.T.);
#4138=EDGE_CURVE('',#3469,#3468,#3181,.T.);
#4139=EDGE_CURVE('',#3470,#3469,#3182,.T.);
#4140=EDGE_CURVE('',#3467,#3470,#1901,.T.);
#4141=EDGE_CURVE('',#3471,#3472,#1902,.T.);
#4142=EDGE_CURVE('',#3472,#3473,#1903,.T.);
#4143=EDGE_CURVE('',#3474,#3473,#1904,.T.);
#4144=EDGE_CURVE('',#3471,#3474,#1905,.T.);
#4145=EDGE_CURVE('',#3475,#3476,#274,.T.);
#4146=EDGE_CURVE('',#3476,#3475,#1906,.T.);
#4147=EDGE_CURVE('',#3470,#3468,#275,.T.);
#4148=EDGE_CURVE('',#3477,#3477,#3183,.T.);
#4149=EDGE_CURVE('',#3477,#3469,#1907,.T.);
#4150=EDGE_CURVE('',#3476,#3475,#3184,.T.);
#4151=EDGE_CURVE('',#3478,#3478,#3185,.T.);
#4152=EDGE_CURVE('',#3479,#3479,#3186,.T.);
#4153=EDGE_CURVE('',#3479,#3478,#1908,.T.);
#4154=EDGE_CURVE('',#3480,#3471,#1909,.T.);
#4155=EDGE_CURVE('',#3481,#3474,#1910,.T.);
#4156=EDGE_CURVE('',#3480,#3481,#1911,.T.);
#4157=EDGE_CURVE('',#3472,#3480,#1912,.T.);
#4158=EDGE_CURVE('',#3473,#3481,#1913,.T.);
#4159=EDGE_CURVE('',#3482,#3483,#1914,.T.);
#4160=EDGE_CURVE('',#3482,#3484,#1915,.T.);
#4161=EDGE_CURVE('',#3485,#3484,#1916,.T.);
#4162=EDGE_CURVE('',#3483,#3485,#1917,.T.);
#4163=EDGE_CURVE('',#3486,#3482,#1918,.T.);
#4164=EDGE_CURVE('',#3486,#3487,#1919,.T.);
#4165=EDGE_CURVE('',#3484,#3487,#1920,.T.);
#4166=EDGE_CURVE('',#3488,#3486,#1921,.T.);
#4167=EDGE_CURVE('',#3488,#3489,#1922,.T.);
#4168=EDGE_CURVE('',#3487,#3489,#1923,.T.);
#4169=EDGE_CURVE('',#3490,#3488,#1924,.T.);
#4170=EDGE_CURVE('',#3490,#3491,#1925,.T.);
#4171=EDGE_CURVE('',#3489,#3491,#1926,.T.);
#4172=EDGE_CURVE('',#3492,#3490,#1927,.T.);
#4173=EDGE_CURVE('',#3492,#3493,#1928,.T.);
#4174=EDGE_CURVE('',#3491,#3493,#1929,.T.);
#4175=EDGE_CURVE('',#3494,#3492,#1930,.T.);
#4176=EDGE_CURVE('',#3494,#3495,#1931,.T.);
#4177=EDGE_CURVE('',#3493,#3495,#1932,.T.);
#4178=EDGE_CURVE('',#3496,#3494,#1933,.T.);
#4179=EDGE_CURVE('',#3496,#3497,#1934,.T.);
#4180=EDGE_CURVE('',#3495,#3497,#1935,.T.);
#4181=EDGE_CURVE('',#3498,#3496,#1936,.T.);
#4182=EDGE_CURVE('',#3498,#3499,#1937,.T.);
#4183=EDGE_CURVE('',#3497,#3499,#1938,.T.);
#4184=EDGE_CURVE('',#3500,#3498,#1939,.T.);
#4185=EDGE_CURVE('',#3501,#3500,#1940,.T.);
#4186=EDGE_CURVE('',#3499,#3501,#1941,.T.);
#4187=EDGE_CURVE('',#3502,#3503,#1942,.T.);
#4188=EDGE_CURVE('',#3502,#3504,#1943,.T.);
#4189=EDGE_CURVE('',#3505,#3504,#1944,.T.);
#4190=EDGE_CURVE('',#3503,#3505,#1945,.T.);
#4191=EDGE_CURVE('',#3506,#3502,#1946,.T.);
#4192=EDGE_CURVE('',#3506,#3507,#1947,.T.);
#4193=EDGE_CURVE('',#3504,#3507,#1948,.T.);
#4194=EDGE_CURVE('',#3508,#3506,#1949,.T.);
#4195=EDGE_CURVE('',#3508,#3509,#1950,.T.);
#4196=EDGE_CURVE('',#3507,#3509,#1951,.T.);
#4197=EDGE_CURVE('',#3510,#3508,#1952,.T.);
#4198=EDGE_CURVE('',#3510,#3511,#1953,.T.);
#4199=EDGE_CURVE('',#3509,#3511,#1954,.T.);
#4200=EDGE_CURVE('',#3512,#3510,#1955,.T.);
#4201=EDGE_CURVE('',#3512,#3513,#1956,.T.);
#4202=EDGE_CURVE('',#3511,#3513,#1957,.T.);
#4203=EDGE_CURVE('',#3514,#3512,#1958,.T.);
#4204=EDGE_CURVE('',#3514,#3515,#1959,.T.);
#4205=EDGE_CURVE('',#3513,#3515,#1960,.T.);
#4206=EDGE_CURVE('',#3516,#3514,#1961,.T.);
#4207=EDGE_CURVE('',#3516,#3517,#1962,.T.);
#4208=EDGE_CURVE('',#3515,#3517,#1963,.T.);
#4209=EDGE_CURVE('',#3518,#3516,#1964,.T.);
#4210=EDGE_CURVE('',#3518,#3519,#1965,.T.);
#4211=EDGE_CURVE('',#3517,#3519,#1966,.T.);
#4212=EDGE_CURVE('',#3520,#3518,#1967,.T.);
#4213=EDGE_CURVE('',#3521,#3520,#1968,.T.);
#4214=EDGE_CURVE('',#3519,#3521,#1969,.T.);
#4215=EDGE_CURVE('',#3522,#3523,#1970,.T.);
#4216=EDGE_CURVE('',#3522,#3524,#1971,.T.);
#4217=EDGE_CURVE('',#3525,#3524,#1972,.T.);
#4218=EDGE_CURVE('',#3523,#3525,#1973,.T.);
#4219=EDGE_CURVE('',#3526,#3522,#1974,.T.);
#4220=EDGE_CURVE('',#3526,#3527,#1975,.T.);
#4221=EDGE_CURVE('',#3524,#3527,#1976,.T.);
#4222=EDGE_CURVE('',#3528,#3526,#1977,.T.);
#4223=EDGE_CURVE('',#3528,#3529,#1978,.T.);
#4224=EDGE_CURVE('',#3527,#3529,#1979,.T.);
#4225=EDGE_CURVE('',#3530,#3528,#1980,.T.);
#4226=EDGE_CURVE('',#3530,#3531,#1981,.T.);
#4227=EDGE_CURVE('',#3529,#3531,#1982,.T.);
#4228=EDGE_CURVE('',#3532,#3530,#1983,.T.);
#4229=EDGE_CURVE('',#3532,#3533,#1984,.T.);
#4230=EDGE_CURVE('',#3531,#3533,#1985,.T.);
#4231=EDGE_CURVE('',#3534,#3532,#1986,.T.);
#4232=EDGE_CURVE('',#3534,#3535,#1987,.T.);
#4233=EDGE_CURVE('',#3533,#3535,#1988,.T.);
#4234=EDGE_CURVE('',#3536,#3534,#1989,.T.);
#4235=EDGE_CURVE('',#3536,#3537,#1990,.T.);
#4236=EDGE_CURVE('',#3535,#3537,#1991,.T.);
#4237=EDGE_CURVE('',#3538,#3536,#1992,.T.);
#4238=EDGE_CURVE('',#3538,#3539,#1993,.T.);
#4239=EDGE_CURVE('',#3537,#3539,#1994,.T.);
#4240=EDGE_CURVE('',#3540,#3538,#1995,.T.);
#4241=EDGE_CURVE('',#3541,#3540,#1996,.T.);
#4242=EDGE_CURVE('',#3539,#3541,#1997,.T.);
#4243=EDGE_CURVE('',#3542,#3543,#1998,.T.);
#4244=EDGE_CURVE('',#3542,#3544,#1999,.T.);
#4245=EDGE_CURVE('',#3545,#3544,#2000,.T.);
#4246=EDGE_CURVE('',#3543,#3545,#2001,.T.);
#4247=EDGE_CURVE('',#3546,#3542,#2002,.T.);
#4248=EDGE_CURVE('',#3546,#3547,#2003,.T.);
#4249=EDGE_CURVE('',#3544,#3547,#2004,.T.);
#4250=EDGE_CURVE('',#3548,#3546,#2005,.T.);
#4251=EDGE_CURVE('',#3548,#3549,#2006,.T.);
#4252=EDGE_CURVE('',#3547,#3549,#2007,.T.);
#4253=EDGE_CURVE('',#3550,#3548,#2008,.T.);
#4254=EDGE_CURVE('',#3550,#3551,#2009,.T.);
#4255=EDGE_CURVE('',#3549,#3551,#2010,.T.);
#4256=EDGE_CURVE('',#3552,#3550,#2011,.T.);
#4257=EDGE_CURVE('',#3552,#3553,#2012,.T.);
#4258=EDGE_CURVE('',#3551,#3553,#2013,.T.);
#4259=EDGE_CURVE('',#3554,#3552,#2014,.T.);
#4260=EDGE_CURVE('',#3554,#3555,#2015,.T.);
#4261=EDGE_CURVE('',#3553,#3555,#2016,.T.);
#4262=EDGE_CURVE('',#3556,#3554,#2017,.T.);
#4263=EDGE_CURVE('',#3556,#3557,#2018,.T.);
#4264=EDGE_CURVE('',#3555,#3557,#2019,.T.);
#4265=EDGE_CURVE('',#3558,#3556,#2020,.T.);
#4266=EDGE_CURVE('',#3558,#3559,#2021,.T.);
#4267=EDGE_CURVE('',#3557,#3559,#2022,.T.);
#4268=EDGE_CURVE('',#3560,#3558,#2023,.T.);
#4269=EDGE_CURVE('',#3561,#3560,#2024,.T.);
#4270=EDGE_CURVE('',#3559,#3561,#2025,.T.);
#4271=EDGE_CURVE('',#3562,#3562,#3187,.T.);
#4272=EDGE_CURVE('',#3562,#3563,#2026,.T.);
#4273=EDGE_CURVE('',#3563,#3563,#3188,.T.);
#4274=EDGE_CURVE('',#3500,#3564,#2027,.T.);
#4275=EDGE_CURVE('',#3564,#3565,#2028,.T.);
#4276=EDGE_CURVE('',#3501,#3565,#2029,.T.);
#4277=EDGE_CURVE('',#3566,#3485,#2030,.T.);
#4278=EDGE_CURVE('',#3567,#3566,#2031,.T.);
#4279=EDGE_CURVE('',#3567,#3483,#2032,.T.);
#4280=EDGE_CURVE('',#3520,#3567,#2033,.T.);
#4281=EDGE_CURVE('',#3521,#3566,#2034,.T.);
#4282=EDGE_CURVE('',#3568,#3505,#2035,.T.);
#4283=EDGE_CURVE('',#3569,#3568,#2036,.T.);
#4284=EDGE_CURVE('',#3569,#3503,#2037,.T.);
#4285=EDGE_CURVE('',#3540,#3569,#2038,.T.);
#4286=EDGE_CURVE('',#3541,#3568,#2039,.T.);
#4287=EDGE_CURVE('',#3570,#3525,#2040,.T.);
#4288=EDGE_CURVE('',#3571,#3570,#2041,.T.);
#4289=EDGE_CURVE('',#3571,#3523,#2042,.T.);
#4290=EDGE_CURVE('',#3560,#3571,#2043,.T.);
#4291=EDGE_CURVE('',#3561,#3570,#2044,.T.);
#4292=EDGE_CURVE('',#3565,#3545,#2045,.T.);
#4293=EDGE_CURVE('',#3564,#3543,#2046,.T.);
#4294=EDGE_CURVE('',#3572,#3572,#3189,.T.);
#4295=EDGE_CURVE('',#3572,#3573,#2047,.T.);
#4296=EDGE_CURVE('',#3573,#3573,#3190,.T.);
#4297=EDGE_CURVE('',#3574,#3574,#3191,.T.);
#4298=EDGE_CURVE('',#3575,#3575,#3192,.T.);
#4299=EDGE_CURVE('',#3575,#3576,#2048,.T.);
#4300=EDGE_CURVE('',#3576,#3576,#3193,.T.);
#4301=EDGE_CURVE('',#3577,#3577,#3194,.T.);
#4302=EDGE_CURVE('',#3578,#3578,#3195,.T.);
#4303=EDGE_CURVE('',#3578,#3579,#2049,.T.);
#4304=EDGE_CURVE('',#3579,#3579,#3196,.T.);
#4305=EDGE_CURVE('',#3580,#3580,#3197,.T.);
#4306=EDGE_CURVE('',#3581,#3581,#3198,.T.);
#4307=EDGE_CURVE('',#3581,#3582,#2050,.T.);
#4308=EDGE_CURVE('',#3582,#3582,#3199,.T.);
#4309=EDGE_CURVE('',#3583,#3583,#3200,.T.);
#4310=EDGE_CURVE('',#3584,#3584,#3201,.T.);
#4311=EDGE_CURVE('',#3584,#3574,#2051,.T.);
#4312=EDGE_CURVE('',#3585,#3585,#3202,.T.);
#4313=EDGE_CURVE('',#3585,#3577,#2052,.T.);
#4314=EDGE_CURVE('',#3586,#3586,#3203,.T.);
#4315=EDGE_CURVE('',#3586,#3580,#2053,.T.);
#4316=EDGE_CURVE('',#3587,#3587,#3204,.T.);
#4317=EDGE_CURVE('',#3587,#3583,#2054,.T.);
#4318=EDGE_CURVE('',#3588,#3589,#2055,.T.);
#4319=EDGE_CURVE('',#3589,#3590,#2056,.T.);
#4320=EDGE_CURVE('',#3591,#3590,#2057,.T.);
#4321=EDGE_CURVE('',#3588,#3591,#2058,.T.);
#4322=EDGE_CURVE('',#3592,#3588,#2059,.T.);
#4323=EDGE_CURVE('',#3593,#3591,#2060,.T.);
#4324=EDGE_CURVE('',#3592,#3593,#2061,.T.);
#4325=EDGE_CURVE('',#3594,#3592,#2062,.T.);
#4326=EDGE_CURVE('',#3595,#3593,#2063,.T.);
#4327=EDGE_CURVE('',#3594,#3595,#2064,.T.);
#4328=EDGE_CURVE('',#3596,#3594,#2065,.T.);
#4329=EDGE_CURVE('',#3597,#3595,#2066,.T.);
#4330=EDGE_CURVE('',#3596,#3597,#2067,.T.);
#4331=EDGE_CURVE('',#3598,#3596,#2068,.T.);
#4332=EDGE_CURVE('',#3599,#3597,#2069,.T.);
#4333=EDGE_CURVE('',#3598,#3599,#2070,.T.);
#4334=EDGE_CURVE('',#3600,#3598,#2071,.T.);
#4335=EDGE_CURVE('',#3601,#3599,#2072,.T.);
#4336=EDGE_CURVE('',#3600,#3601,#2073,.T.);
#4337=EDGE_CURVE('',#3602,#3600,#2074,.T.);
#4338=EDGE_CURVE('',#3603,#3601,#2075,.T.);
#4339=EDGE_CURVE('',#3602,#3603,#2076,.T.);
#4340=EDGE_CURVE('',#3604,#3602,#2077,.T.);
#4341=EDGE_CURVE('',#3605,#3603,#2078,.T.);
#4342=EDGE_CURVE('',#3604,#3605,#2079,.T.);
#4343=EDGE_CURVE('',#3606,#3604,#2080,.T.);
#4344=EDGE_CURVE('',#3607,#3605,#2081,.T.);
#4345=EDGE_CURVE('',#3606,#3607,#2082,.T.);
#4346=EDGE_CURVE('',#3608,#3606,#2083,.T.);
#4347=EDGE_CURVE('',#3609,#3607,#2084,.T.);
#4348=EDGE_CURVE('',#3608,#3609,#2085,.T.);
#4349=EDGE_CURVE('',#3610,#3608,#2086,.T.);
#4350=EDGE_CURVE('',#3611,#3609,#2087,.T.);
#4351=EDGE_CURVE('',#3610,#3611,#2088,.T.);
#4352=EDGE_CURVE('',#3589,#3610,#2089,.T.);
#4353=EDGE_CURVE('',#3590,#3611,#2090,.T.);
#4354=EDGE_CURVE('',#3612,#3613,#2091,.T.);
#4355=EDGE_CURVE('',#3613,#3614,#2092,.T.);
#4356=EDGE_CURVE('',#3614,#3615,#2093,.T.);
#4357=EDGE_CURVE('',#3612,#3615,#2094,.T.);
#4358=EDGE_CURVE('',#3613,#3616,#2095,.T.);
#4359=EDGE_CURVE('',#3616,#3617,#2096,.T.);
#4360=EDGE_CURVE('',#3617,#3614,#2097,.T.);
#4361=EDGE_CURVE('',#3616,#3618,#2098,.T.);
#4362=EDGE_CURVE('',#3618,#3619,#2099,.T.);
#4363=EDGE_CURVE('',#3619,#3617,#2100,.T.);
#4364=EDGE_CURVE('',#3618,#3620,#2101,.T.);
#4365=EDGE_CURVE('',#3620,#3621,#2102,.T.);
#4366=EDGE_CURVE('',#3621,#3619,#2103,.T.);
#4367=EDGE_CURVE('',#3620,#3622,#2104,.T.);
#4368=EDGE_CURVE('',#3622,#3623,#2105,.T.);
#4369=EDGE_CURVE('',#3623,#3621,#2106,.T.);
#4370=EDGE_CURVE('',#3622,#3612,#2107,.T.);
#4371=EDGE_CURVE('',#3615,#3623,#2108,.T.);
#4372=EDGE_CURVE('',#3624,#3624,#3205,.T.);
#4373=EDGE_CURVE('',#3625,#3625,#3206,.T.);
#4374=EDGE_CURVE('',#3624,#3626,#2109,.T.);
#4375=EDGE_CURVE('',#3626,#3626,#3207,.T.);
#4376=EDGE_CURVE('',#3627,#3627,#3208,.T.);
#4377=EDGE_CURVE('',#3628,#3628,#3209,.T.);
#4378=EDGE_CURVE('',#3628,#3627,#2110,.T.);
#4379=EDGE_CURVE('',#3629,#3629,#3210,.T.);
#4380=EDGE_CURVE('',#3629,#3628,#2111,.T.);
#4381=EDGE_CURVE('',#3630,#3630,#3211,.T.);
#4382=EDGE_CURVE('',#3630,#3629,#2112,.T.);
#4383=EDGE_CURVE('',#3631,#3631,#3212,.T.);
#4384=EDGE_CURVE('',#3632,#3632,#3213,.F.);
#4385=EDGE_CURVE('',#3632,#3631,#2113,.T.);
#4386=EDGE_CURVE('',#3625,#3632,#2114,.T.);
#4387=EDGE_CURVE('',#3633,#3633,#3214,.T.);
#4388=EDGE_CURVE('',#3634,#3634,#3215,.T.);
#4389=EDGE_CURVE('',#3634,#3633,#2115,.T.);
#4390=EDGE_CURVE('',#3635,#3635,#3216,.T.);
#4391=EDGE_CURVE('',#3635,#3634,#2116,.T.);
#4392=EDGE_CURVE('',#3636,#3636,#3217,.T.);
#4393=EDGE_CURVE('',#3636,#3635,#2117,.T.);
#4394=EDGE_CURVE('',#3637,#3637,#3218,.T.);
#4395=EDGE_CURVE('',#3638,#3638,#3219,.F.);
#4396=EDGE_CURVE('',#3638,#3637,#2118,.T.);
#4397=EDGE_CURVE('',#3639,#3639,#3220,.F.);
#4398=EDGE_CURVE('',#3639,#3638,#2119,.T.);
#4399=EDGE_CURVE('',#3640,#3640,#3221,.T.);
#4400=EDGE_CURVE('',#3640,#3639,#2120,.T.);
#4401=EDGE_CURVE('',#3641,#3642,#2121,.T.);
#4402=EDGE_CURVE('',#3642,#3643,#2122,.T.);
#4403=EDGE_CURVE('',#3643,#3644,#2123,.T.);
#4404=EDGE_CURVE('',#3641,#3644,#2124,.T.);
#4405=EDGE_CURVE('',#3642,#3645,#2125,.T.);
#4406=EDGE_CURVE('',#3645,#3646,#2126,.T.);
#4407=EDGE_CURVE('',#3646,#3643,#2127,.T.);
#4408=EDGE_CURVE('',#3645,#3647,#2128,.T.);
#4409=EDGE_CURVE('',#3647,#3648,#2129,.T.);
#4410=EDGE_CURVE('',#3648,#3646,#2130,.T.);
#4411=EDGE_CURVE('',#3647,#3649,#2131,.T.);
#4412=EDGE_CURVE('',#3649,#3650,#2132,.T.);
#4413=EDGE_CURVE('',#3650,#3648,#2133,.T.);
#4414=EDGE_CURVE('',#3649,#3651,#2134,.T.);
#4415=EDGE_CURVE('',#3651,#3652,#2135,.T.);
#4416=EDGE_CURVE('',#3652,#3650,#2136,.T.);
#4417=EDGE_CURVE('',#3651,#3641,#2137,.T.);
#4418=EDGE_CURVE('',#3644,#3652,#2138,.T.);
#4419=EDGE_CURVE('',#3653,#3654,#2139,.T.);
#4420=EDGE_CURVE('',#3655,#3653,#2140,.T.);
#4421=EDGE_CURVE('',#3656,#3655,#2141,.T.);
#4422=EDGE_CURVE('',#3654,#3656,#2142,.T.);
#4423=EDGE_CURVE('',#3655,#3657,#2143,.T.);
#4424=EDGE_CURVE('',#3658,#3657,#2144,.T.);
#4425=EDGE_CURVE('',#3656,#3658,#2145,.T.);
#4426=EDGE_CURVE('',#3657,#3659,#2146,.T.);
#4427=EDGE_CURVE('',#3659,#3660,#2147,.T.);
#4428=EDGE_CURVE('',#3660,#3658,#2148,.T.);
#4429=EDGE_CURVE('',#3661,#3661,#3222,.T.);
#4430=EDGE_CURVE('',#3662,#3653,#2149,.T.);
#4431=EDGE_CURVE('',#3663,#3662,#2150,.T.);
#4432=EDGE_CURVE('',#3663,#3664,#2151,.T.);
#4433=EDGE_CURVE('',#3665,#3664,#2152,.T.);
#4434=EDGE_CURVE('',#3665,#3666,#2153,.T.);
#4435=EDGE_CURVE('',#3666,#3667,#2154,.T.);
#4436=EDGE_CURVE('',#3667,#3659,#2155,.T.);
#4437=EDGE_CURVE('',#3667,#3668,#2156,.T.);
#4438=EDGE_CURVE('',#3668,#3660,#2157,.T.);
#4439=EDGE_CURVE('',#3669,#3666,#2158,.T.);
#4440=EDGE_CURVE('',#3668,#3669,#2159,.T.);
#4441=EDGE_CURVE('',#3670,#3669,#2160,.T.);
#4442=EDGE_CURVE('',#3671,#3670,#2161,.T.);
#4443=EDGE_CURVE('',#3671,#3672,#2162,.T.);
#4444=EDGE_CURVE('',#3673,#3672,#2163,.T.);
#4445=EDGE_CURVE('',#3673,#3654,#2164,.T.);
#4446=EDGE_CURVE('',#3670,#3665,#2165,.T.);
#4447=EDGE_CURVE('',#3664,#3674,#2166,.T.);
#4448=EDGE_CURVE('',#3674,#3675,#276,.T.);
#4449=EDGE_CURVE('',#3675,#3671,#2167,.T.);
#4450=EDGE_CURVE('',#3676,#3674,#3223,.F.);
#4451=EDGE_CURVE('',#3676,#3661,#2168,.T.);
#4452=EDGE_CURVE('',#3677,#3676,#3224,.F.);
#4453=EDGE_CURVE('',#3678,#3677,#277,.T.);
#4454=EDGE_CURVE('',#3675,#3678,#3225,.F.);
#4455=EDGE_CURVE('',#3677,#3663,#2169,.T.);
#4456=EDGE_CURVE('',#3672,#3678,#2170,.T.);
#4457=EDGE_CURVE('',#3662,#3673,#2171,.T.);
#4458=EDGE_CURVE('',#3679,#3679,#3226,.T.);
#4459=EDGE_CURVE('',#3679,#3680,#2172,.T.);
#4460=EDGE_CURVE('',#3680,#3680,#3227,.T.);
#4461=EDGE_CURVE('',#3680,#3681,#2173,.T.);
#4462=EDGE_CURVE('',#3681,#3681,#3228,.T.);
#4463=EDGE_CURVE('',#3682,#3682,#3229,.T.);
#4464=EDGE_CURVE('',#3682,#3683,#2174,.T.);
#4465=EDGE_CURVE('',#3683,#3683,#3230,.T.);
#4466=EDGE_CURVE('',#3684,#3684,#3231,.T.);
#4467=EDGE_CURVE('',#3684,#3685,#2175,.T.);
#4468=EDGE_CURVE('',#3685,#3685,#3232,.T.);
#4469=EDGE_CURVE('',#3686,#3687,#2176,.T.);
#4470=EDGE_CURVE('',#3688,#3686,#2177,.T.);
#4471=EDGE_CURVE('',#3689,#3688,#2178,.T.);
#4472=EDGE_CURVE('',#3687,#3689,#2179,.T.);
#4473=EDGE_CURVE('',#3688,#3690,#2180,.T.);
#4474=EDGE_CURVE('',#3691,#3690,#2181,.T.);
#4475=EDGE_CURVE('',#3689,#3691,#2182,.T.);
#4476=EDGE_CURVE('',#3692,#3693,#2183,.T.);
#4477=EDGE_CURVE('',#3692,#3691,#2184,.T.);
#4478=EDGE_CURVE('',#3690,#3693,#2185,.T.);
#4479=EDGE_CURVE('',#3694,#3687,#2186,.T.);
#4480=EDGE_CURVE('',#3694,#3695,#2187,.T.);
#4481=EDGE_CURVE('',#3695,#3686,#2188,.T.);
#4482=EDGE_CURVE('',#3693,#3696,#2189,.T.);
#4483=EDGE_CURVE('',#3696,#3697,#2190,.T.);
#4484=EDGE_CURVE('',#3697,#3698,#2191,.T.);
#4485=EDGE_CURVE('',#3699,#3698,#2192,.T.);
#4486=EDGE_CURVE('',#3692,#3699,#2193,.T.);
#4487=EDGE_CURVE('',#3700,#3700,#3233,.T.);
#4488=EDGE_CURVE('',#3700,#3701,#2194,.T.);
#4489=EDGE_CURVE('',#3701,#3701,#3234,.T.);
#4490=EDGE_CURVE('',#3702,#3702,#3235,.T.);
#4491=EDGE_CURVE('',#3702,#3703,#2195,.T.);
#4492=EDGE_CURVE('',#3703,#3703,#3236,.T.);
#4493=EDGE_CURVE('',#3704,#3704,#3237,.T.);
#4494=EDGE_CURVE('',#3704,#3705,#2196,.T.);
#4495=EDGE_CURVE('',#3705,#3705,#3238,.T.);
#4496=EDGE_CURVE('',#3706,#3707,#2197,.T.);
#4497=EDGE_CURVE('',#3708,#3706,#3239,.T.);
#4498=EDGE_CURVE('',#3709,#3708,#2198,.T.);
#4499=EDGE_CURVE('',#3709,#3707,#3240,.T.);
#4500=EDGE_CURVE('',#3708,#3706,#2199,.T.);
#4501=EDGE_CURVE('',#3695,#3710,#2200,.T.);
#4502=EDGE_CURVE('',#3710,#3711,#2201,.T.);
#4503=EDGE_CURVE('',#3711,#3712,#2202,.T.);
#4504=EDGE_CURVE('',#3713,#3712,#3241,.T.);
#4505=EDGE_CURVE('',#3713,#3707,#2203,.T.);
#4506=EDGE_CURVE('',#3709,#3696,#2204,.T.);
#4507=EDGE_CURVE('',#3714,#3714,#3242,.T.);
#4508=EDGE_CURVE('',#3715,#3715,#3243,.T.);
#4509=EDGE_CURVE('',#3716,#3716,#3244,.T.);
#4510=EDGE_CURVE('',#3717,#3717,#3245,.T.);
#4511=EDGE_CURVE('',#3714,#3718,#2205,.T.);
#4512=EDGE_CURVE('',#3718,#3718,#3246,.T.);
#4513=EDGE_CURVE('',#3713,#3719,#2206,.T.);
#4514=EDGE_CURVE('',#3719,#3720,#2207,.T.);
#4515=EDGE_CURVE('',#3720,#3712,#2208,.T.);
#4516=EDGE_CURVE('',#3721,#3711,#2209,.T.);
#4517=EDGE_CURVE('',#3722,#3721,#2210,.T.);
#4518=EDGE_CURVE('',#3723,#3722,#2211,.T.);
#4519=EDGE_CURVE('',#3724,#3723,#2212,.T.);
#4520=EDGE_CURVE('',#3696,#3724,#2213,.T.);
#4521=EDGE_CURVE('',#3717,#3725,#2214,.T.);
#4522=EDGE_CURVE('',#3725,#3725,#3247,.T.);
#4523=EDGE_CURVE('',#3719,#3720,#3248,.T.);
#4524=EDGE_CURVE('',#3716,#3726,#2215,.T.);
#4525=EDGE_CURVE('',#3726,#3726,#3249,.T.);
#4526=EDGE_CURVE('',#3715,#3727,#2216,.T.);
#4527=EDGE_CURVE('',#3727,#3727,#3250,.T.);
#4528=EDGE_CURVE('',#3711,#3728,#2217,.T.);
#4529=EDGE_CURVE('',#3729,#3728,#2218,.T.);
#4530=EDGE_CURVE('',#3721,#3729,#2219,.T.);
#4531=EDGE_CURVE('',#3724,#3730,#2220,.T.);
#4532=EDGE_CURVE('',#3697,#3730,#2221,.T.);
#4533=EDGE_CURVE('',#3723,#3731,#2222,.T.);
#4534=EDGE_CURVE('',#3730,#3731,#2223,.T.);
#4535=EDGE_CURVE('',#3732,#3729,#2224,.T.);
#4536=EDGE_CURVE('',#3722,#3732,#2225,.T.);
#4537=EDGE_CURVE('',#3731,#3732,#2226,.T.);
#4538=EDGE_CURVE('',#3697,#3728,#2227,.T.);
#4539=EDGE_CURVE('',#3728,#3733,#2228,.T.);
#4540=EDGE_CURVE('',#3698,#3733,#2229,.T.);
#4541=EDGE_CURVE('',#3734,#3699,#2230,.T.);
#4542=EDGE_CURVE('',#3735,#3734,#2231,.T.);
#4543=EDGE_CURVE('',#3735,#3694,#2232,.T.);
#4544=EDGE_CURVE('',#3710,#3735,#2233,.T.);
#4545=EDGE_CURVE('',#3733,#3734,#2234,.T.);
#4546=EDGE_CURVE('',#3736,#3736,#3251,.T.);
#4547=EDGE_CURVE('',#3736,#3737,#2235,.T.);
#4548=EDGE_CURVE('',#3737,#3737,#3252,.T.);
#4549=EDGE_CURVE('',#3738,#3738,#3253,.T.);
#4550=EDGE_CURVE('',#3738,#3739,#2236,.T.);
#4551=EDGE_CURVE('',#3739,#3739,#3254,.T.);
#4552=EDGE_CURVE('',#3740,#3740,#3255,.T.);
#4553=EDGE_CURVE('',#3740,#3741,#2237,.T.);
#4554=EDGE_CURVE('',#3741,#3741,#3256,.T.);
#4555=EDGE_CURVE('',#3742,#3742,#3257,.T.);
#4556=EDGE_CURVE('',#3742,#3743,#2238,.T.);
#4557=EDGE_CURVE('',#3743,#3743,#3258,.T.);
#4558=EDGE_CURVE('',#3744,#3744,#3259,.T.);
#4559=EDGE_CURVE('',#3745,#3745,#3260,.T.);
#4560=EDGE_CURVE('',#3746,#3746,#3261,.T.);
#4561=EDGE_CURVE('',#3746,#3744,#2239,.T.);
#4562=EDGE_CURVE('',#3745,#3747,#2240,.T.);
#4563=EDGE_CURVE('',#3747,#3747,#3262,.T.);
#4564=EDGE_CURVE('',#3748,#3748,#3263,.T.);
#4565=EDGE_CURVE('',#3748,#3749,#2241,.T.);
#4566=EDGE_CURVE('',#3749,#3749,#3264,.T.);
#4567=EDGE_CURVE('',#3750,#3750,#3265,.T.);
#4568=EDGE_CURVE('',#3750,#3751,#2242,.T.);
#4569=EDGE_CURVE('',#3751,#3751,#3266,.T.);
#4570=EDGE_CURVE('',#3752,#3752,#3267,.T.);
#4571=EDGE_CURVE('',#3752,#3753,#2243,.T.);
#4572=EDGE_CURVE('',#3753,#3753,#3268,.T.);
#4573=EDGE_CURVE('',#3754,#3754,#3269,.T.);
#4574=EDGE_CURVE('',#3754,#3755,#2244,.T.);
#4575=EDGE_CURVE('',#3755,#3755,#3270,.T.);
#4576=EDGE_CURVE('',#3756,#3757,#2245,.T.);
#4577=EDGE_CURVE('',#3757,#3758,#2246,.T.);
#4578=EDGE_CURVE('',#3759,#3758,#2247,.T.);
#4579=EDGE_CURVE('',#3756,#3759,#2248,.T.);
#4580=EDGE_CURVE('',#3760,#3756,#2249,.T.);
#4581=EDGE_CURVE('',#3761,#3759,#2250,.T.);
#4582=EDGE_CURVE('',#3760,#3761,#2251,.T.);
#4583=EDGE_CURVE('',#3762,#3760,#2252,.T.);
#4584=EDGE_CURVE('',#3763,#3761,#2253,.T.);
#4585=EDGE_CURVE('',#3762,#3763,#2254,.T.);
#4586=EDGE_CURVE('',#3757,#3762,#2255,.T.);
#4587=EDGE_CURVE('',#3758,#3763,#2256,.T.);
#4588=EDGE_CURVE('',#3764,#3765,#2257,.T.);
#4589=EDGE_CURVE('',#3765,#3766,#2258,.T.);
#4590=EDGE_CURVE('',#3767,#3766,#2259,.T.);
#4591=EDGE_CURVE('',#3764,#3767,#2260,.T.);
#4592=EDGE_CURVE('',#3768,#3764,#2261,.T.);
#4593=EDGE_CURVE('',#3769,#3767,#2262,.T.);
#4594=EDGE_CURVE('',#3768,#3769,#2263,.T.);
#4595=EDGE_CURVE('',#3770,#3768,#2264,.T.);
#4596=EDGE_CURVE('',#3771,#3769,#2265,.T.);
#4597=EDGE_CURVE('',#3770,#3771,#2266,.T.);
#4598=EDGE_CURVE('',#3765,#3770,#2267,.T.);
#4599=EDGE_CURVE('',#3766,#3771,#2268,.T.);
#4600=EDGE_CURVE('',#3772,#3772,#3271,.T.);
#4601=EDGE_CURVE('',#3772,#3773,#2269,.T.);
#4602=EDGE_CURVE('',#3773,#3773,#3272,.T.);
#4603=EDGE_CURVE('',#3774,#3774,#3273,.T.);
#4604=EDGE_CURVE('',#3774,#3775,#2270,.T.);
#4605=EDGE_CURVE('',#3775,#3775,#3274,.T.);
#4606=EDGE_CURVE('',#3776,#3777,#2271,.T.);
#4607=EDGE_CURVE('',#3776,#3777,#3275,.T.);
#4608=EDGE_CURVE('',#3778,#3776,#2272,.T.);
#4609=EDGE_CURVE('',#3779,#3778,#3276,.T.);
#4610=EDGE_CURVE('',#3779,#3780,#2273,.T.);
#4611=EDGE_CURVE('',#3780,#3780,#3277,.T.);
#4612=EDGE_CURVE('',#3781,#3779,#3278,.T.);
#4613=EDGE_CURVE('',#3777,#3781,#2274,.T.);
#4614=EDGE_CURVE('',#3782,#3783,#2275,.T.);
#4615=EDGE_CURVE('',#3782,#3783,#3279,.T.);
#4616=EDGE_CURVE('',#3784,#3782,#2276,.T.);
#4617=EDGE_CURVE('',#3785,#3784,#3280,.T.);
#4618=EDGE_CURVE('',#3785,#3786,#2277,.T.);
#4619=EDGE_CURVE('',#3786,#3786,#3281,.T.);
#4620=EDGE_CURVE('',#3787,#3785,#3282,.T.);
#4621=EDGE_CURVE('',#3783,#3787,#2278,.T.);
#4622=EDGE_CURVE('',#3788,#3789,#2279,.T.);
#4623=EDGE_CURVE('',#3788,#3789,#3283,.T.);
#4624=EDGE_CURVE('',#3790,#3788,#2280,.T.);
#4625=EDGE_CURVE('',#3791,#3790,#3284,.T.);
#4626=EDGE_CURVE('',#3791,#3792,#2281,.T.);
#4627=EDGE_CURVE('',#3792,#3792,#3285,.T.);
#4628=EDGE_CURVE('',#3793,#3791,#3286,.T.);
#4629=EDGE_CURVE('',#3789,#3793,#2282,.T.);
#4630=EDGE_CURVE('',#3794,#3795,#2283,.T.);
#4631=EDGE_CURVE('',#3794,#3795,#3287,.T.);
#4632=EDGE_CURVE('',#3796,#3794,#2284,.T.);
#4633=EDGE_CURVE('',#3797,#3796,#3288,.T.);
#4634=EDGE_CURVE('',#3797,#3798,#2285,.T.);
#4635=EDGE_CURVE('',#3798,#3798,#3289,.T.);
#4636=EDGE_CURVE('',#3799,#3797,#3290,.T.);
#4637=EDGE_CURVE('',#3795,#3799,#2286,.T.);
#4638=EDGE_CURVE('',#3781,#3790,#2287,.T.);
#4639=EDGE_CURVE('',#3793,#3800,#2288,.T.);
#4640=EDGE_CURVE('',#3801,#3800,#2289,.T.);
#4641=EDGE_CURVE('',#3801,#3802,#2290,.T.);
#4642=EDGE_CURVE('',#3803,#3802,#2291,.T.);
#4643=EDGE_CURVE('',#3803,#3778,#2292,.T.);
#4644=EDGE_CURVE('',#3787,#3796,#2293,.T.);
#4645=EDGE_CURVE('',#3799,#3804,#2294,.T.);
#4646=EDGE_CURVE('',#3805,#3804,#2295,.T.);
#4647=EDGE_CURVE('',#3806,#3805,#2296,.T.);
#4648=EDGE_CURVE('',#3807,#3806,#2297,.T.);
#4649=EDGE_CURVE('',#3807,#3784,#2298,.T.);
#4650=EDGE_CURVE('',#3800,#3808,#2299,.T.);
#4651=EDGE_CURVE('',#3808,#3809,#2300,.T.);
#4652=EDGE_CURVE('',#3809,#3810,#2301,.T.);
#4653=EDGE_CURVE('',#3810,#3811,#2302,.T.);
#4654=EDGE_CURVE('',#3811,#3807,#2303,.T.);
#4655=EDGE_CURVE('',#3806,#3812,#2304,.T.);
#4656=EDGE_CURVE('',#3812,#3813,#2305,.T.);
#4657=EDGE_CURVE('',#3813,#3814,#2306,.T.);
#4658=EDGE_CURVE('',#3814,#3815,#2307,.T.);
#4659=EDGE_CURVE('',#3815,#3801,#2308,.T.);
#4660=EDGE_CURVE('',#3816,#3803,#2309,.T.);
#4661=EDGE_CURVE('',#3808,#3816,#2310,.T.);
#4662=EDGE_CURVE('',#3817,#3816,#2311,.T.);
#4663=EDGE_CURVE('',#3809,#3817,#2312,.T.);
#4664=EDGE_CURVE('',#3818,#3817,#2313,.T.);
#4665=EDGE_CURVE('',#3810,#3818,#2314,.T.);
#4666=EDGE_CURVE('',#3819,#3818,#2315,.T.);
#4667=EDGE_CURVE('',#3811,#3819,#2316,.T.);
#4668=EDGE_CURVE('',#3804,#3819,#2317,.T.);
#4669=EDGE_CURVE('',#3820,#3805,#2318,.T.);
#4670=EDGE_CURVE('',#3812,#3820,#2319,.T.);
#4671=EDGE_CURVE('',#3821,#3820,#2320,.T.);
#4672=EDGE_CURVE('',#3813,#3821,#2321,.T.);
#4673=EDGE_CURVE('',#3822,#3821,#2322,.T.);
#4674=EDGE_CURVE('',#3814,#3822,#2323,.T.);
#4675=EDGE_CURVE('',#3823,#3822,#2324,.T.);
#4676=EDGE_CURVE('',#3815,#3823,#2325,.T.);
#4677=EDGE_CURVE('',#3802,#3823,#2326,.T.);
#4678=EDGE_CURVE('',#3824,#3825,#2327,.T.);
#4679=EDGE_CURVE('',#3825,#3826,#2328,.T.);
#4680=EDGE_CURVE('',#3827,#3826,#2329,.T.);
#4681=EDGE_CURVE('',#3824,#3827,#2330,.T.);
#4682=EDGE_CURVE('',#3828,#3824,#2331,.T.);
#4683=EDGE_CURVE('',#3829,#3827,#2332,.T.);
#4684=EDGE_CURVE('',#3828,#3829,#2333,.T.);
#4685=EDGE_CURVE('',#3830,#3828,#2334,.T.);
#4686=EDGE_CURVE('',#3831,#3829,#2335,.T.);
#4687=EDGE_CURVE('',#3830,#3831,#2336,.T.);
#4688=EDGE_CURVE('',#3832,#3830,#2337,.T.);
#4689=EDGE_CURVE('',#3833,#3831,#2338,.T.);
#4690=EDGE_CURVE('',#3832,#3833,#2339,.T.);
#4691=EDGE_CURVE('',#3834,#3832,#2340,.T.);
#4692=EDGE_CURVE('',#3835,#3833,#2341,.T.);
#4693=EDGE_CURVE('',#3834,#3835,#2342,.T.);
#4694=EDGE_CURVE('',#3836,#3834,#2343,.T.);
#4695=EDGE_CURVE('',#3837,#3835,#2344,.T.);
#4696=EDGE_CURVE('',#3836,#3837,#2345,.T.);
#4697=EDGE_CURVE('',#3838,#3836,#2346,.T.);
#4698=EDGE_CURVE('',#3839,#3837,#2347,.T.);
#4699=EDGE_CURVE('',#3838,#3839,#2348,.T.);
#4700=EDGE_CURVE('',#3825,#3838,#2349,.T.);
#4701=EDGE_CURVE('',#3826,#3839,#2350,.T.);
#4702=EDGE_CURVE('',#3840,#3841,#2351,.T.);
#4703=EDGE_CURVE('',#3840,#3842,#2352,.T.);
#4704=EDGE_CURVE('',#3843,#3842,#2353,.T.);
#4705=EDGE_CURVE('',#3841,#3843,#2354,.T.);
#4706=EDGE_CURVE('',#3841,#3844,#2355,.T.);
#4707=EDGE_CURVE('',#3845,#3843,#2356,.T.);
#4708=EDGE_CURVE('',#3844,#3845,#2357,.T.);
#4709=EDGE_CURVE('',#3844,#3846,#2358,.T.);
#4710=EDGE_CURVE('',#3847,#3845,#2359,.T.);
#4711=EDGE_CURVE('',#3846,#3847,#2360,.T.);
#4712=EDGE_CURVE('',#3846,#3848,#2361,.T.);
#4713=EDGE_CURVE('',#3849,#3847,#2362,.T.);
#4714=EDGE_CURVE('',#3848,#3849,#2363,.T.);
#4715=EDGE_CURVE('',#3848,#3850,#2364,.T.);
#4716=EDGE_CURVE('',#3851,#3849,#2365,.T.);
#4717=EDGE_CURVE('',#3850,#3851,#2366,.T.);
#4718=EDGE_CURVE('',#3850,#3852,#2367,.T.);
#4719=EDGE_CURVE('',#3853,#3851,#2368,.T.);
#4720=EDGE_CURVE('',#3852,#3853,#2369,.T.);
#4721=EDGE_CURVE('',#3852,#3854,#2370,.T.);
#4722=EDGE_CURVE('',#3855,#3853,#2371,.T.);
#4723=EDGE_CURVE('',#3854,#3855,#2372,.T.);
#4724=EDGE_CURVE('',#3854,#3840,#2373,.T.);
#4725=EDGE_CURVE('',#3842,#3855,#2374,.T.);
#4726=EDGE_CURVE('',#3856,#3857,#2375,.T.);
#4727=EDGE_CURVE('',#3857,#3858,#2376,.T.);
#4728=EDGE_CURVE('',#3858,#3859,#2377,.T.);
#4729=EDGE_CURVE('',#3856,#3859,#2378,.T.);
#4730=EDGE_CURVE('',#3857,#3860,#2379,.T.);
#4731=EDGE_CURVE('',#3860,#3861,#2380,.T.);
#4732=EDGE_CURVE('',#3861,#3858,#2381,.T.);
#4733=EDGE_CURVE('',#3860,#3862,#2382,.T.);
#4734=EDGE_CURVE('',#3862,#3863,#2383,.T.);
#4735=EDGE_CURVE('',#3863,#3861,#2384,.T.);
#4736=EDGE_CURVE('',#3862,#3864,#2385,.T.);
#4737=EDGE_CURVE('',#3864,#3865,#2386,.T.);
#4738=EDGE_CURVE('',#3865,#3863,#2387,.T.);
#4739=EDGE_CURVE('',#3864,#3866,#2388,.T.);
#4740=EDGE_CURVE('',#3866,#3867,#2389,.T.);
#4741=EDGE_CURVE('',#3867,#3865,#2390,.T.);
#4742=EDGE_CURVE('',#3866,#3856,#2391,.T.);
#4743=EDGE_CURVE('',#3859,#3867,#2392,.T.);
#4744=EDGE_CURVE('',#3868,#3868,#3291,.T.);
#4745=EDGE_CURVE('',#3869,#3869,#3292,.T.);
#4746=EDGE_CURVE('',#3870,#3870,#3293,.T.);
#4747=EDGE_CURVE('',#3870,#3869,#2393,.T.);
#4748=EDGE_CURVE('',#3871,#3871,#3294,.T.);
#4749=EDGE_CURVE('',#3871,#3870,#2394,.T.);
#4750=EDGE_CURVE('',#3872,#3872,#3295,.T.);
#4751=EDGE_CURVE('',#3872,#3871,#2395,.T.);
#4752=EDGE_CURVE('',#3873,#3873,#3296,.T.);
#4753=EDGE_CURVE('',#3874,#3874,#3297,.F.);
#4754=EDGE_CURVE('',#3874,#3873,#2396,.T.);
#4755=EDGE_CURVE('',#3868,#3874,#2397,.T.);
#4756=EDGE_CURVE('',#3875,#3875,#3298,.T.);
#4757=EDGE_CURVE('',#3876,#3876,#3299,.T.);
#4758=EDGE_CURVE('',#3876,#3875,#2398,.T.);
#4759=EDGE_CURVE('',#3877,#3877,#3300,.T.);
#4760=EDGE_CURVE('',#3877,#3876,#2399,.T.);
#4761=EDGE_CURVE('',#3878,#3878,#3301,.T.);
#4762=EDGE_CURVE('',#3878,#3877,#2400,.T.);
#4763=EDGE_CURVE('',#3879,#3879,#3302,.T.);
#4764=EDGE_CURVE('',#3880,#3880,#3303,.F.);
#4765=EDGE_CURVE('',#3880,#3879,#2401,.T.);
#4766=EDGE_CURVE('',#3881,#3881,#3304,.F.);
#4767=EDGE_CURVE('',#3881,#3880,#2402,.T.);
#4768=EDGE_CURVE('',#3882,#3882,#3305,.T.);
#4769=EDGE_CURVE('',#3882,#3881,#2403,.T.);
#4770=EDGE_CURVE('',#3883,#3884,#2404,.T.);
#4771=EDGE_CURVE('',#3884,#3885,#2405,.T.);
#4772=EDGE_CURVE('',#3885,#3886,#2406,.T.);
#4773=EDGE_CURVE('',#3883,#3886,#2407,.T.);
#4774=EDGE_CURVE('',#3884,#3887,#2408,.T.);
#4775=EDGE_CURVE('',#3887,#3888,#2409,.T.);
#4776=EDGE_CURVE('',#3888,#3885,#2410,.T.);
#4777=EDGE_CURVE('',#3887,#3889,#2411,.T.);
#4778=EDGE_CURVE('',#3889,#3890,#2412,.T.);
#4779=EDGE_CURVE('',#3890,#3888,#2413,.T.);
#4780=EDGE_CURVE('',#3889,#3891,#2414,.T.);
#4781=EDGE_CURVE('',#3891,#3892,#2415,.T.);
#4782=EDGE_CURVE('',#3892,#3890,#2416,.T.);
#4783=EDGE_CURVE('',#3891,#3893,#2417,.T.);
#4784=EDGE_CURVE('',#3893,#3894,#2418,.T.);
#4785=EDGE_CURVE('',#3894,#3892,#2419,.T.);
#4786=EDGE_CURVE('',#3893,#3883,#2420,.T.);
#4787=EDGE_CURVE('',#3886,#3894,#2421,.T.);
#4788=ORIENTED_EDGE('',*,*,#3895,.F.);
#4789=ORIENTED_EDGE('',*,*,#3896,.T.);
#4790=ORIENTED_EDGE('',*,*,#3897,.F.);
#4791=ORIENTED_EDGE('',*,*,#3896,.F.);
#4792=ORIENTED_EDGE('',*,*,#3895,.T.);
#4793=ORIENTED_EDGE('',*,*,#3898,.F.);
#4794=ORIENTED_EDGE('',*,*,#3899,.T.);
#4795=ORIENTED_EDGE('',*,*,#3900,.F.);
#4796=ORIENTED_EDGE('',*,*,#3899,.F.);
#4797=ORIENTED_EDGE('',*,*,#3898,.T.);
#4798=ORIENTED_EDGE('',*,*,#3901,.F.);
#4799=ORIENTED_EDGE('',*,*,#3902,.T.);
#4800=ORIENTED_EDGE('',*,*,#3903,.F.);
#4801=ORIENTED_EDGE('',*,*,#3902,.F.);
#4802=ORIENTED_EDGE('',*,*,#3901,.T.);
#4803=ORIENTED_EDGE('',*,*,#3904,.F.);
#4804=ORIENTED_EDGE('',*,*,#3905,.T.);
#4805=ORIENTED_EDGE('',*,*,#3906,.F.);
#4806=ORIENTED_EDGE('',*,*,#3905,.F.);
#4807=ORIENTED_EDGE('',*,*,#3904,.T.);
#4808=ORIENTED_EDGE('',*,*,#3907,.F.);
#4809=ORIENTED_EDGE('',*,*,#3908,.T.);
#4810=ORIENTED_EDGE('',*,*,#3909,.F.);
#4811=ORIENTED_EDGE('',*,*,#3908,.F.);
#4812=ORIENTED_EDGE('',*,*,#3910,.T.);
#4813=ORIENTED_EDGE('',*,*,#3911,.T.);
#4814=ORIENTED_EDGE('',*,*,#3912,.F.);
#4815=ORIENTED_EDGE('',*,*,#3913,.F.);
#4816=ORIENTED_EDGE('',*,*,#3914,.T.);
#4817=ORIENTED_EDGE('',*,*,#3913,.T.);
#4818=ORIENTED_EDGE('',*,*,#3915,.F.);
#4819=ORIENTED_EDGE('',*,*,#3916,.F.);
#4820=ORIENTED_EDGE('',*,*,#3917,.T.);
#4821=ORIENTED_EDGE('',*,*,#3916,.T.);
#4822=ORIENTED_EDGE('',*,*,#3918,.F.);
#4823=ORIENTED_EDGE('',*,*,#3919,.F.);
#4824=ORIENTED_EDGE('',*,*,#3920,.T.);
#4825=ORIENTED_EDGE('',*,*,#3919,.T.);
#4826=ORIENTED_EDGE('',*,*,#3921,.F.);
#4827=ORIENTED_EDGE('',*,*,#3911,.F.);
#4828=ORIENTED_EDGE('',*,*,#3921,.T.);
#4829=ORIENTED_EDGE('',*,*,#3918,.T.);
#4830=ORIENTED_EDGE('',*,*,#3915,.T.);
#4831=ORIENTED_EDGE('',*,*,#3912,.T.);
#4832=ORIENTED_EDGE('',*,*,#3897,.T.);
#4833=ORIENTED_EDGE('',*,*,#3900,.T.);
#4834=ORIENTED_EDGE('',*,*,#3903,.T.);
#4835=ORIENTED_EDGE('',*,*,#3906,.T.);
#4836=ORIENTED_EDGE('',*,*,#3909,.T.);
#4837=ORIENTED_EDGE('',*,*,#3920,.F.);
#4838=ORIENTED_EDGE('',*,*,#3910,.F.);
#4839=ORIENTED_EDGE('',*,*,#3914,.F.);
#4840=ORIENTED_EDGE('',*,*,#3917,.F.);
#4841=ORIENTED_EDGE('',*,*,#3907,.T.);
#4842=ORIENTED_EDGE('',*,*,#3922,.T.);
#4843=ORIENTED_EDGE('',*,*,#3923,.T.);
#4844=ORIENTED_EDGE('',*,*,#3924,.F.);
#4845=ORIENTED_EDGE('',*,*,#3925,.F.);
#4846=ORIENTED_EDGE('',*,*,#3926,.T.);
#4847=ORIENTED_EDGE('',*,*,#3925,.T.);
#4848=ORIENTED_EDGE('',*,*,#3927,.F.);
#4849=ORIENTED_EDGE('',*,*,#3928,.F.);
#4850=ORIENTED_EDGE('',*,*,#3929,.T.);
#4851=ORIENTED_EDGE('',*,*,#3928,.T.);
#4852=ORIENTED_EDGE('',*,*,#3930,.F.);
#4853=ORIENTED_EDGE('',*,*,#3931,.F.);
#4854=ORIENTED_EDGE('',*,*,#3932,.T.);
#4855=ORIENTED_EDGE('',*,*,#3931,.T.);
#4856=ORIENTED_EDGE('',*,*,#3933,.F.);
#4857=ORIENTED_EDGE('',*,*,#3923,.F.);
#4858=ORIENTED_EDGE('',*,*,#3933,.T.);
#4859=ORIENTED_EDGE('',*,*,#3930,.T.);
#4860=ORIENTED_EDGE('',*,*,#3927,.T.);
#4861=ORIENTED_EDGE('',*,*,#3924,.T.);
#4862=ORIENTED_EDGE('',*,*,#3932,.F.);
#4863=ORIENTED_EDGE('',*,*,#3922,.F.);
#4864=ORIENTED_EDGE('',*,*,#3926,.F.);
#4865=ORIENTED_EDGE('',*,*,#3929,.F.);
#4866=ORIENTED_EDGE('',*,*,#3934,.T.);
#4867=ORIENTED_EDGE('',*,*,#3935,.T.);
#4868=ORIENTED_EDGE('',*,*,#3936,.F.);
#4869=ORIENTED_EDGE('',*,*,#3937,.F.);
#4870=ORIENTED_EDGE('',*,*,#3938,.T.);
#4871=ORIENTED_EDGE('',*,*,#3937,.T.);
#4872=ORIENTED_EDGE('',*,*,#3939,.F.);
#4873=ORIENTED_EDGE('',*,*,#3940,.F.);
#4874=ORIENTED_EDGE('',*,*,#3941,.T.);
#4875=ORIENTED_EDGE('',*,*,#3940,.T.);
#4876=ORIENTED_EDGE('',*,*,#3942,.F.);
#4877=ORIENTED_EDGE('',*,*,#3943,.F.);
#4878=ORIENTED_EDGE('',*,*,#3944,.T.);
#4879=ORIENTED_EDGE('',*,*,#3943,.T.);
#4880=ORIENTED_EDGE('',*,*,#3945,.F.);
#4881=ORIENTED_EDGE('',*,*,#3935,.F.);
#4882=ORIENTED_EDGE('',*,*,#3945,.T.);
#4883=ORIENTED_EDGE('',*,*,#3942,.T.);
#4884=ORIENTED_EDGE('',*,*,#3939,.T.);
#4885=ORIENTED_EDGE('',*,*,#3936,.T.);
#4886=ORIENTED_EDGE('',*,*,#3944,.F.);
#4887=ORIENTED_EDGE('',*,*,#3934,.F.);
#4888=ORIENTED_EDGE('',*,*,#3938,.F.);
#4889=ORIENTED_EDGE('',*,*,#3941,.F.);
#4890=ORIENTED_EDGE('',*,*,#3946,.F.);
#4891=ORIENTED_EDGE('',*,*,#3947,.T.);
#4892=ORIENTED_EDGE('',*,*,#3948,.F.);
#4893=ORIENTED_EDGE('',*,*,#3947,.F.);
#4894=ORIENTED_EDGE('',*,*,#3949,.T.);
#4895=ORIENTED_EDGE('',*,*,#3950,.T.);
#4896=ORIENTED_EDGE('',*,*,#3951,.F.);
#4897=ORIENTED_EDGE('',*,*,#3952,.F.);
#4898=ORIENTED_EDGE('',*,*,#3953,.T.);
#4899=ORIENTED_EDGE('',*,*,#3952,.T.);
#4900=ORIENTED_EDGE('',*,*,#3954,.F.);
#4901=ORIENTED_EDGE('',*,*,#3955,.F.);
#4902=ORIENTED_EDGE('',*,*,#3956,.T.);
#4903=ORIENTED_EDGE('',*,*,#3955,.T.);
#4904=ORIENTED_EDGE('',*,*,#3957,.F.);
#4905=ORIENTED_EDGE('',*,*,#3958,.F.);
#4906=ORIENTED_EDGE('',*,*,#3959,.T.);
#4907=ORIENTED_EDGE('',*,*,#3958,.T.);
#4908=ORIENTED_EDGE('',*,*,#3960,.F.);
#4909=ORIENTED_EDGE('',*,*,#3950,.F.);
#4910=ORIENTED_EDGE('',*,*,#3960,.T.);
#4911=ORIENTED_EDGE('',*,*,#3957,.T.);
#4912=ORIENTED_EDGE('',*,*,#3954,.T.);
#4913=ORIENTED_EDGE('',*,*,#3951,.T.);
#4914=ORIENTED_EDGE('',*,*,#3948,.T.);
#4915=ORIENTED_EDGE('',*,*,#3959,.F.);
#4916=ORIENTED_EDGE('',*,*,#3949,.F.);
#4917=ORIENTED_EDGE('',*,*,#3953,.F.);
#4918=ORIENTED_EDGE('',*,*,#3956,.F.);
#4919=ORIENTED_EDGE('',*,*,#3946,.T.);
#4920=ORIENTED_EDGE('',*,*,#3961,.F.);
#4921=ORIENTED_EDGE('',*,*,#3962,.T.);
#4922=ORIENTED_EDGE('',*,*,#3963,.F.);
#4923=ORIENTED_EDGE('',*,*,#3962,.F.);
#4924=ORIENTED_EDGE('',*,*,#3964,.F.);
#4925=ORIENTED_EDGE('',*,*,#3965,.T.);
#4926=ORIENTED_EDGE('',*,*,#3966,.F.);
#4927=ORIENTED_EDGE('',*,*,#3965,.F.);
#4928=ORIENTED_EDGE('',*,*,#3967,.F.);
#4929=ORIENTED_EDGE('',*,*,#3968,.T.);
#4930=ORIENTED_EDGE('',*,*,#3969,.F.);
#4931=ORIENTED_EDGE('',*,*,#3968,.F.);
#4932=ORIENTED_EDGE('',*,*,#3970,.F.);
#4933=ORIENTED_EDGE('',*,*,#3971,.T.);
#4934=ORIENTED_EDGE('',*,*,#3972,.F.);
#4935=ORIENTED_EDGE('',*,*,#3971,.F.);
#4936=ORIENTED_EDGE('',*,*,#3973,.F.);
#4937=ORIENTED_EDGE('',*,*,#3974,.T.);
#4938=ORIENTED_EDGE('',*,*,#3975,.F.);
#4939=ORIENTED_EDGE('',*,*,#3974,.F.);
#4940=ORIENTED_EDGE('',*,*,#3976,.F.);
#4941=ORIENTED_EDGE('',*,*,#3977,.T.);
#4942=ORIENTED_EDGE('',*,*,#3978,.F.);
#4943=ORIENTED_EDGE('',*,*,#3977,.F.);
#4944=ORIENTED_EDGE('',*,*,#3979,.F.);
#4945=ORIENTED_EDGE('',*,*,#3980,.T.);
#4946=ORIENTED_EDGE('',*,*,#3981,.F.);
#4947=ORIENTED_EDGE('',*,*,#3980,.F.);
#4948=ORIENTED_EDGE('',*,*,#3982,.F.);
#4949=ORIENTED_EDGE('',*,*,#3983,.T.);
#4950=ORIENTED_EDGE('',*,*,#3984,.F.);
#4951=ORIENTED_EDGE('',*,*,#3983,.F.);
#4952=ORIENTED_EDGE('',*,*,#3985,.F.);
#4953=ORIENTED_EDGE('',*,*,#3986,.F.);
#4954=ORIENTED_EDGE('',*,*,#3987,.F.);
#4955=ORIENTED_EDGE('',*,*,#3988,.F.);
#4956=ORIENTED_EDGE('',*,*,#3989,.F.);
#4957=ORIENTED_EDGE('',*,*,#3990,.F.);
#4958=ORIENTED_EDGE('',*,*,#3991,.F.);
#4959=ORIENTED_EDGE('',*,*,#3992,.T.);
#4960=ORIENTED_EDGE('',*,*,#3993,.F.);
#4961=ORIENTED_EDGE('',*,*,#3992,.F.);
#4962=ORIENTED_EDGE('',*,*,#3994,.F.);
#4963=ORIENTED_EDGE('',*,*,#3986,.T.);
#4964=ORIENTED_EDGE('',*,*,#3987,.T.);
#4965=ORIENTED_EDGE('',*,*,#3994,.T.);
#4966=ORIENTED_EDGE('',*,*,#3991,.T.);
#4967=ORIENTED_EDGE('',*,*,#3995,.F.);
#4968=ORIENTED_EDGE('',*,*,#3996,.T.);
#4969=ORIENTED_EDGE('',*,*,#3997,.T.);
#4970=ORIENTED_EDGE('',*,*,#3998,.F.);
#4971=ORIENTED_EDGE('',*,*,#3999,.F.);
#4972=ORIENTED_EDGE('',*,*,#3982,.T.);
#4973=ORIENTED_EDGE('',*,*,#3979,.T.);
#4974=ORIENTED_EDGE('',*,*,#3976,.T.);
#4975=ORIENTED_EDGE('',*,*,#3973,.T.);
#4976=ORIENTED_EDGE('',*,*,#3970,.T.);
#4977=ORIENTED_EDGE('',*,*,#3967,.T.);
#4978=ORIENTED_EDGE('',*,*,#3964,.T.);
#4979=ORIENTED_EDGE('',*,*,#3961,.T.);
#4980=ORIENTED_EDGE('',*,*,#3990,.T.);
#4981=ORIENTED_EDGE('',*,*,#4000,.F.);
#4982=ORIENTED_EDGE('',*,*,#4001,.T.);
#4983=ORIENTED_EDGE('',*,*,#3995,.T.);
#4984=ORIENTED_EDGE('',*,*,#3988,.T.);
#4985=ORIENTED_EDGE('',*,*,#3999,.T.);
#4986=ORIENTED_EDGE('',*,*,#4002,.F.);
#4987=ORIENTED_EDGE('',*,*,#4003,.F.);
#4988=ORIENTED_EDGE('',*,*,#3985,.T.);
#4989=ORIENTED_EDGE('',*,*,#4003,.T.);
#4990=ORIENTED_EDGE('',*,*,#4004,.F.);
#4991=ORIENTED_EDGE('',*,*,#4005,.F.);
#4992=ORIENTED_EDGE('',*,*,#4006,.T.);
#4993=ORIENTED_EDGE('',*,*,#4000,.T.);
#4994=ORIENTED_EDGE('',*,*,#3989,.T.);
#4995=ORIENTED_EDGE('',*,*,#3993,.T.);
#4996=ORIENTED_EDGE('',*,*,#3984,.T.);
#4997=ORIENTED_EDGE('',*,*,#3981,.T.);
#4998=ORIENTED_EDGE('',*,*,#3978,.T.);
#4999=ORIENTED_EDGE('',*,*,#3975,.T.);
#5000=ORIENTED_EDGE('',*,*,#3972,.T.);
#5001=ORIENTED_EDGE('',*,*,#3969,.T.);
#5002=ORIENTED_EDGE('',*,*,#3966,.T.);
#5003=ORIENTED_EDGE('',*,*,#3963,.T.);
#5004=ORIENTED_EDGE('',*,*,#4007,.T.);
#5005=ORIENTED_EDGE('',*,*,#4005,.T.);
#5006=ORIENTED_EDGE('',*,*,#4008,.F.);
#5007=ORIENTED_EDGE('',*,*,#3997,.F.);
#5008=ORIENTED_EDGE('',*,*,#3998,.T.);
#5009=ORIENTED_EDGE('',*,*,#4008,.T.);
#5010=ORIENTED_EDGE('',*,*,#4004,.T.);
#5011=ORIENTED_EDGE('',*,*,#4002,.T.);
#5012=ORIENTED_EDGE('',*,*,#3996,.F.);
#5013=ORIENTED_EDGE('',*,*,#4001,.F.);
#5014=ORIENTED_EDGE('',*,*,#4006,.F.);
#5015=ORIENTED_EDGE('',*,*,#4007,.F.);
#5016=ORIENTED_EDGE('',*,*,#4009,.F.);
#5017=ORIENTED_EDGE('',*,*,#4010,.T.);
#5018=ORIENTED_EDGE('',*,*,#4011,.F.);
#5019=ORIENTED_EDGE('',*,*,#4010,.F.);
#5020=ORIENTED_EDGE('',*,*,#4012,.T.);
#5021=ORIENTED_EDGE('',*,*,#4013,.T.);
#5022=ORIENTED_EDGE('',*,*,#4014,.F.);
#5023=ORIENTED_EDGE('',*,*,#4015,.F.);
#5024=ORIENTED_EDGE('',*,*,#4016,.T.);
#5025=ORIENTED_EDGE('',*,*,#4015,.T.);
#5026=ORIENTED_EDGE('',*,*,#4017,.F.);
#5027=ORIENTED_EDGE('',*,*,#4018,.F.);
#5028=ORIENTED_EDGE('',*,*,#4011,.T.);
#5029=ORIENTED_EDGE('',*,*,#4019,.T.);
#5030=ORIENTED_EDGE('',*,*,#4018,.T.);
#5031=ORIENTED_EDGE('',*,*,#4020,.F.);
#5032=ORIENTED_EDGE('',*,*,#4021,.F.);
#5033=ORIENTED_EDGE('',*,*,#4022,.T.);
#5034=ORIENTED_EDGE('',*,*,#4021,.T.);
#5035=ORIENTED_EDGE('',*,*,#4023,.F.);
#5036=ORIENTED_EDGE('',*,*,#4013,.F.);
#5037=ORIENTED_EDGE('',*,*,#4009,.T.);
#5038=ORIENTED_EDGE('',*,*,#4023,.T.);
#5039=ORIENTED_EDGE('',*,*,#4020,.T.);
#5040=ORIENTED_EDGE('',*,*,#4017,.T.);
#5041=ORIENTED_EDGE('',*,*,#4014,.T.);
#5042=ORIENTED_EDGE('',*,*,#4022,.F.);
#5043=ORIENTED_EDGE('',*,*,#4012,.F.);
#5044=ORIENTED_EDGE('',*,*,#4016,.F.);
#5045=ORIENTED_EDGE('',*,*,#4019,.F.);
#5046=ORIENTED_EDGE('',*,*,#4024,.F.);
#5047=ORIENTED_EDGE('',*,*,#4025,.T.);
#5048=ORIENTED_EDGE('',*,*,#4026,.F.);
#5049=ORIENTED_EDGE('',*,*,#4025,.F.);
#5050=ORIENTED_EDGE('',*,*,#4027,.T.);
#5051=ORIENTED_EDGE('',*,*,#4028,.T.);
#5052=ORIENTED_EDGE('',*,*,#4029,.F.);
#5053=ORIENTED_EDGE('',*,*,#4030,.F.);
#5054=ORIENTED_EDGE('',*,*,#4031,.T.);
#5055=ORIENTED_EDGE('',*,*,#4030,.T.);
#5056=ORIENTED_EDGE('',*,*,#4032,.F.);
#5057=ORIENTED_EDGE('',*,*,#4033,.F.);
#5058=ORIENTED_EDGE('',*,*,#4026,.T.);
#5059=ORIENTED_EDGE('',*,*,#4034,.T.);
#5060=ORIENTED_EDGE('',*,*,#4033,.T.);
#5061=ORIENTED_EDGE('',*,*,#4035,.F.);
#5062=ORIENTED_EDGE('',*,*,#4036,.F.);
#5063=ORIENTED_EDGE('',*,*,#4037,.T.);
#5064=ORIENTED_EDGE('',*,*,#4036,.T.);
#5065=ORIENTED_EDGE('',*,*,#4038,.F.);
#5066=ORIENTED_EDGE('',*,*,#4028,.F.);
#5067=ORIENTED_EDGE('',*,*,#4024,.T.);
#5068=ORIENTED_EDGE('',*,*,#4038,.T.);
#5069=ORIENTED_EDGE('',*,*,#4035,.T.);
#5070=ORIENTED_EDGE('',*,*,#4032,.T.);
#5071=ORIENTED_EDGE('',*,*,#4029,.T.);
#5072=ORIENTED_EDGE('',*,*,#4037,.F.);
#5073=ORIENTED_EDGE('',*,*,#4027,.F.);
#5074=ORIENTED_EDGE('',*,*,#4031,.F.);
#5075=ORIENTED_EDGE('',*,*,#4034,.F.);
#5076=ORIENTED_EDGE('',*,*,#4039,.F.);
#5077=ORIENTED_EDGE('',*,*,#4040,.T.);
#5078=ORIENTED_EDGE('',*,*,#4041,.F.);
#5079=ORIENTED_EDGE('',*,*,#4040,.F.);
#5080=ORIENTED_EDGE('',*,*,#4042,.F.);
#5081=ORIENTED_EDGE('',*,*,#4043,.T.);
#5082=ORIENTED_EDGE('',*,*,#4044,.F.);
#5083=ORIENTED_EDGE('',*,*,#4043,.F.);
#5084=ORIENTED_EDGE('',*,*,#4045,.F.);
#5085=ORIENTED_EDGE('',*,*,#4046,.T.);
#5086=ORIENTED_EDGE('',*,*,#4047,.F.);
#5087=ORIENTED_EDGE('',*,*,#4046,.F.);
#5088=ORIENTED_EDGE('',*,*,#4048,.F.);
#5089=ORIENTED_EDGE('',*,*,#4049,.T.);
#5090=ORIENTED_EDGE('',*,*,#4050,.F.);
#5091=ORIENTED_EDGE('',*,*,#4049,.F.);
#5092=ORIENTED_EDGE('',*,*,#4048,.T.);
#5093=ORIENTED_EDGE('',*,*,#4045,.T.);
#5094=ORIENTED_EDGE('',*,*,#4051,.T.);
#5095=ORIENTED_EDGE('',*,*,#4041,.T.);
#5096=ORIENTED_EDGE('',*,*,#4044,.T.);
#5097=ORIENTED_EDGE('',*,*,#4050,.T.);
#5098=ORIENTED_EDGE('',*,*,#4051,.F.);
#5099=ORIENTED_EDGE('',*,*,#4052,.T.);
#5100=ORIENTED_EDGE('',*,*,#4053,.T.);
#5101=ORIENTED_EDGE('',*,*,#4052,.F.);
#5102=ORIENTED_EDGE('',*,*,#4047,.T.);
#5103=ORIENTED_EDGE('',*,*,#4053,.F.);
#5104=ORIENTED_EDGE('',*,*,#4039,.T.);
#5105=ORIENTED_EDGE('',*,*,#4042,.T.);
#5106=ORIENTED_EDGE('',*,*,#4054,.F.);
#5107=ORIENTED_EDGE('',*,*,#4055,.T.);
#5108=ORIENTED_EDGE('',*,*,#4056,.T.);
#5109=ORIENTED_EDGE('',*,*,#4055,.F.);
#5110=ORIENTED_EDGE('',*,*,#4057,.F.);
#5111=ORIENTED_EDGE('',*,*,#4058,.T.);
#5112=ORIENTED_EDGE('',*,*,#4059,.T.);
#5113=ORIENTED_EDGE('',*,*,#4058,.F.);
#5114=ORIENTED_EDGE('',*,*,#4057,.T.);
#5115=ORIENTED_EDGE('',*,*,#4054,.T.);
#5116=ORIENTED_EDGE('',*,*,#4059,.F.);
#5117=ORIENTED_EDGE('',*,*,#4056,.F.);
#5118=ORIENTED_EDGE('',*,*,#4060,.F.);
#5119=ORIENTED_EDGE('',*,*,#4061,.T.);
#5120=ORIENTED_EDGE('',*,*,#4062,.F.);
#5121=ORIENTED_EDGE('',*,*,#4061,.F.);
#5122=ORIENTED_EDGE('',*,*,#4063,.F.);
#5123=ORIENTED_EDGE('',*,*,#4064,.T.);
#5124=ORIENTED_EDGE('',*,*,#4065,.F.);
#5125=ORIENTED_EDGE('',*,*,#4064,.F.);
#5126=ORIENTED_EDGE('',*,*,#4066,.F.);
#5127=ORIENTED_EDGE('',*,*,#4067,.T.);
#5128=ORIENTED_EDGE('',*,*,#4068,.F.);
#5129=ORIENTED_EDGE('',*,*,#4067,.F.);
#5130=ORIENTED_EDGE('',*,*,#4066,.T.);
#5131=ORIENTED_EDGE('',*,*,#4069,.F.);
#5132=ORIENTED_EDGE('',*,*,#4070,.F.);
#5133=ORIENTED_EDGE('',*,*,#4071,.T.);
#5134=ORIENTED_EDGE('',*,*,#4072,.T.);
#5135=ORIENTED_EDGE('',*,*,#4071,.F.);
#5136=ORIENTED_EDGE('',*,*,#4072,.F.);
#5137=ORIENTED_EDGE('',*,*,#4073,.F.);
#5138=ORIENTED_EDGE('',*,*,#4069,.T.);
#5139=ORIENTED_EDGE('',*,*,#4074,.T.);
#5140=ORIENTED_EDGE('',*,*,#4073,.T.);
#5141=ORIENTED_EDGE('',*,*,#4074,.F.);
#5142=ORIENTED_EDGE('',*,*,#4075,.F.);
#5143=ORIENTED_EDGE('',*,*,#4076,.T.);
#5144=ORIENTED_EDGE('',*,*,#4077,.T.);
#5145=ORIENTED_EDGE('',*,*,#4076,.F.);
#5146=ORIENTED_EDGE('',*,*,#4075,.T.);
#5147=ORIENTED_EDGE('',*,*,#4062,.T.);
#5148=ORIENTED_EDGE('',*,*,#4065,.T.);
#5149=ORIENTED_EDGE('',*,*,#4068,.T.);
#5150=ORIENTED_EDGE('',*,*,#4077,.F.);
#5151=ORIENTED_EDGE('',*,*,#4060,.T.);
#5152=ORIENTED_EDGE('',*,*,#4063,.T.);
#5153=ORIENTED_EDGE('',*,*,#4070,.T.);
#5154=ORIENTED_EDGE('',*,*,#4078,.T.);
#5155=ORIENTED_EDGE('',*,*,#4079,.F.);
#5156=ORIENTED_EDGE('',*,*,#4080,.F.);
#5157=ORIENTED_EDGE('',*,*,#4081,.F.);
#5158=ORIENTED_EDGE('',*,*,#4078,.F.);
#5159=ORIENTED_EDGE('',*,*,#4082,.T.);
#5160=ORIENTED_EDGE('',*,*,#4080,.T.);
#5161=ORIENTED_EDGE('',*,*,#4082,.F.);
#5162=ORIENTED_EDGE('',*,*,#4081,.T.);
#5163=ORIENTED_EDGE('',*,*,#4083,.T.);
#5164=ORIENTED_EDGE('',*,*,#4084,.T.);
#5165=ORIENTED_EDGE('',*,*,#4083,.F.);
#5166=ORIENTED_EDGE('',*,*,#4085,.F.);
#5167=ORIENTED_EDGE('',*,*,#4086,.T.);
#5168=ORIENTED_EDGE('',*,*,#4079,.T.);
#5169=ORIENTED_EDGE('',*,*,#4086,.F.);
#5170=ORIENTED_EDGE('',*,*,#4085,.T.);
#5171=ORIENTED_EDGE('',*,*,#4084,.F.);
#5172=ORIENTED_EDGE('',*,*,#4087,.F.);
#5173=ORIENTED_EDGE('',*,*,#4088,.T.);
#5174=ORIENTED_EDGE('',*,*,#4089,.T.);
#5175=ORIENTED_EDGE('',*,*,#4088,.F.);
#5176=ORIENTED_EDGE('',*,*,#4090,.F.);
#5177=ORIENTED_EDGE('',*,*,#4091,.T.);
#5178=ORIENTED_EDGE('',*,*,#4092,.T.);
#5179=ORIENTED_EDGE('',*,*,#4091,.F.);
#5180=ORIENTED_EDGE('',*,*,#4090,.T.);
#5181=ORIENTED_EDGE('',*,*,#4087,.T.);
#5182=ORIENTED_EDGE('',*,*,#4092,.F.);
#5183=ORIENTED_EDGE('',*,*,#4089,.F.);
#5184=ORIENTED_EDGE('',*,*,#4093,.T.);
#5185=ORIENTED_EDGE('',*,*,#4094,.F.);
#5186=ORIENTED_EDGE('',*,*,#4095,.F.);
#5187=ORIENTED_EDGE('',*,*,#4096,.F.);
#5188=ORIENTED_EDGE('',*,*,#4093,.F.);
#5189=ORIENTED_EDGE('',*,*,#4097,.T.);
#5190=ORIENTED_EDGE('',*,*,#4095,.T.);
#5191=ORIENTED_EDGE('',*,*,#4097,.F.);
#5192=ORIENTED_EDGE('',*,*,#4096,.T.);
#5193=ORIENTED_EDGE('',*,*,#4098,.T.);
#5194=ORIENTED_EDGE('',*,*,#4099,.T.);
#5195=ORIENTED_EDGE('',*,*,#4098,.F.);
#5196=ORIENTED_EDGE('',*,*,#4100,.F.);
#5197=ORIENTED_EDGE('',*,*,#4101,.T.);
#5198=ORIENTED_EDGE('',*,*,#4094,.T.);
#5199=ORIENTED_EDGE('',*,*,#4101,.F.);
#5200=ORIENTED_EDGE('',*,*,#4100,.T.);
#5201=ORIENTED_EDGE('',*,*,#4099,.F.);
#5202=ORIENTED_EDGE('',*,*,#4102,.F.);
#5203=ORIENTED_EDGE('',*,*,#4103,.T.);
#5204=ORIENTED_EDGE('',*,*,#4104,.T.);
#5205=ORIENTED_EDGE('',*,*,#4103,.F.);
#5206=ORIENTED_EDGE('',*,*,#4105,.F.);
#5207=ORIENTED_EDGE('',*,*,#4106,.T.);
#5208=ORIENTED_EDGE('',*,*,#4107,.T.);
#5209=ORIENTED_EDGE('',*,*,#4106,.F.);
#5210=ORIENTED_EDGE('',*,*,#4105,.T.);
#5211=ORIENTED_EDGE('',*,*,#4102,.T.);
#5212=ORIENTED_EDGE('',*,*,#4107,.F.);
#5213=ORIENTED_EDGE('',*,*,#4104,.F.);
#5214=ORIENTED_EDGE('',*,*,#4108,.T.);
#5215=ORIENTED_EDGE('',*,*,#4109,.T.);
#5216=ORIENTED_EDGE('',*,*,#4110,.F.);
#5217=ORIENTED_EDGE('',*,*,#4109,.F.);
#5218=ORIENTED_EDGE('',*,*,#4110,.T.);
#5219=ORIENTED_EDGE('',*,*,#4108,.F.);
#5220=ORIENTED_EDGE('',*,*,#4111,.F.);
#5221=ORIENTED_EDGE('',*,*,#4112,.T.);
#5222=ORIENTED_EDGE('',*,*,#4113,.F.);
#5223=ORIENTED_EDGE('',*,*,#4114,.F.);
#5224=ORIENTED_EDGE('',*,*,#4115,.F.);
#5225=ORIENTED_EDGE('',*,*,#4116,.F.);
#5226=ORIENTED_EDGE('',*,*,#4112,.F.);
#5227=ORIENTED_EDGE('',*,*,#4117,.F.);
#5228=ORIENTED_EDGE('',*,*,#4118,.T.);
#5229=ORIENTED_EDGE('',*,*,#4119,.F.);
#5230=ORIENTED_EDGE('',*,*,#4120,.F.);
#5231=ORIENTED_EDGE('',*,*,#4121,.T.);
#5232=ORIENTED_EDGE('',*,*,#4122,.T.);
#5233=ORIENTED_EDGE('',*,*,#4113,.T.);
#5234=ORIENTED_EDGE('',*,*,#4111,.T.);
#5235=ORIENTED_EDGE('',*,*,#4116,.T.);
#5236=ORIENTED_EDGE('',*,*,#4123,.T.);
#5237=ORIENTED_EDGE('',*,*,#4115,.T.);
#5238=ORIENTED_EDGE('',*,*,#4124,.T.);
#5239=ORIENTED_EDGE('',*,*,#4125,.F.);
#5240=ORIENTED_EDGE('',*,*,#4124,.F.);
#5241=ORIENTED_EDGE('',*,*,#4114,.T.);
#5242=ORIENTED_EDGE('',*,*,#4123,.F.);
#5243=ORIENTED_EDGE('',*,*,#4122,.F.);
#5244=ORIENTED_EDGE('',*,*,#4126,.T.);
#5245=ORIENTED_EDGE('',*,*,#4127,.F.);
#5246=ORIENTED_EDGE('',*,*,#4121,.F.);
#5247=ORIENTED_EDGE('',*,*,#4126,.F.);
#5248=ORIENTED_EDGE('',*,*,#4128,.F.);
#5249=ORIENTED_EDGE('',*,*,#4129,.T.);
#5250=ORIENTED_EDGE('',*,*,#4127,.T.);
#5251=ORIENTED_EDGE('',*,*,#4129,.F.);
#5252=ORIENTED_EDGE('',*,*,#4130,.F.);
#5253=ORIENTED_EDGE('',*,*,#4120,.T.);
#5254=ORIENTED_EDGE('',*,*,#4131,.F.);
#5255=ORIENTED_EDGE('',*,*,#4132,.F.);
#5256=ORIENTED_EDGE('',*,*,#4125,.T.);
#5257=ORIENTED_EDGE('',*,*,#4133,.F.);
#5258=ORIENTED_EDGE('',*,*,#4132,.T.);
#5259=ORIENTED_EDGE('',*,*,#4134,.F.);
#5260=ORIENTED_EDGE('',*,*,#4118,.F.);
#5261=ORIENTED_EDGE('',*,*,#4128,.T.);
#5262=ORIENTED_EDGE('',*,*,#4119,.T.);
#5263=ORIENTED_EDGE('',*,*,#4134,.T.);
#5264=ORIENTED_EDGE('',*,*,#4131,.T.);
#5265=ORIENTED_EDGE('',*,*,#4117,.T.);
#5266=ORIENTED_EDGE('',*,*,#4130,.T.);
#5267=ORIENTED_EDGE('',*,*,#4133,.T.);
#5268=ORIENTED_EDGE('',*,*,#4135,.F.);
#5269=ORIENTED_EDGE('',*,*,#4136,.F.);
#5270=ORIENTED_EDGE('',*,*,#4137,.F.);
#5271=ORIENTED_EDGE('',*,*,#4138,.F.);
#5272=ORIENTED_EDGE('',*,*,#4139,.F.);
#5273=ORIENTED_EDGE('',*,*,#4140,.F.);
#5274=ORIENTED_EDGE('',*,*,#4136,.T.);
#5275=ORIENTED_EDGE('',*,*,#4141,.T.);
#5276=ORIENTED_EDGE('',*,*,#4142,.T.);
#5277=ORIENTED_EDGE('',*,*,#4143,.F.);
#5278=ORIENTED_EDGE('',*,*,#4144,.F.);
#5279=ORIENTED_EDGE('',*,*,#4145,.T.);
#5280=ORIENTED_EDGE('',*,*,#4146,.T.);
#5281=ORIENTED_EDGE('',*,*,#4137,.T.);
#5282=ORIENTED_EDGE('',*,*,#4135,.T.);
#5283=ORIENTED_EDGE('',*,*,#4140,.T.);
#5284=ORIENTED_EDGE('',*,*,#4147,.T.);
#5285=ORIENTED_EDGE('',*,*,#4148,.F.);
#5286=ORIENTED_EDGE('',*,*,#4149,.T.);
#5287=ORIENTED_EDGE('',*,*,#4138,.T.);
#5288=ORIENTED_EDGE('',*,*,#4147,.F.);
#5289=ORIENTED_EDGE('',*,*,#4139,.T.);
#5290=ORIENTED_EDGE('',*,*,#4149,.F.);
#5291=ORIENTED_EDGE('',*,*,#4146,.F.);
#5292=ORIENTED_EDGE('',*,*,#4150,.T.);
#5293=ORIENTED_EDGE('',*,*,#4151,.F.);
#5294=ORIENTED_EDGE('',*,*,#4145,.F.);
#5295=ORIENTED_EDGE('',*,*,#4150,.F.);
#5296=ORIENTED_EDGE('',*,*,#4152,.F.);
#5297=ORIENTED_EDGE('',*,*,#4153,.T.);
#5298=ORIENTED_EDGE('',*,*,#4151,.T.);
#5299=ORIENTED_EDGE('',*,*,#4153,.F.);
#5300=ORIENTED_EDGE('',*,*,#4154,.T.);
#5301=ORIENTED_EDGE('',*,*,#4144,.T.);
#5302=ORIENTED_EDGE('',*,*,#4155,.F.);
#5303=ORIENTED_EDGE('',*,*,#4156,.F.);
#5304=ORIENTED_EDGE('',*,*,#4152,.T.);
#5305=ORIENTED_EDGE('',*,*,#4157,.T.);
#5306=ORIENTED_EDGE('',*,*,#4156,.T.);
#5307=ORIENTED_EDGE('',*,*,#4158,.F.);
#5308=ORIENTED_EDGE('',*,*,#4142,.F.);
#5309=ORIENTED_EDGE('',*,*,#4148,.T.);
#5310=ORIENTED_EDGE('',*,*,#4158,.T.);
#5311=ORIENTED_EDGE('',*,*,#4155,.T.);
#5312=ORIENTED_EDGE('',*,*,#4143,.T.);
#5313=ORIENTED_EDGE('',*,*,#4157,.F.);
#5314=ORIENTED_EDGE('',*,*,#4141,.F.);
#5315=ORIENTED_EDGE('',*,*,#4154,.F.);
#5316=ORIENTED_EDGE('',*,*,#4159,.F.);
#5317=ORIENTED_EDGE('',*,*,#4160,.T.);
#5318=ORIENTED_EDGE('',*,*,#4161,.F.);
#5319=ORIENTED_EDGE('',*,*,#4162,.F.);
#5320=ORIENTED_EDGE('',*,*,#4163,.F.);
#5321=ORIENTED_EDGE('',*,*,#4164,.T.);
#5322=ORIENTED_EDGE('',*,*,#4165,.F.);
#5323=ORIENTED_EDGE('',*,*,#4160,.F.);
#5324=ORIENTED_EDGE('',*,*,#4166,.F.);
#5325=ORIENTED_EDGE('',*,*,#4167,.T.);
#5326=ORIENTED_EDGE('',*,*,#4168,.F.);
#5327=ORIENTED_EDGE('',*,*,#4164,.F.);
#5328=ORIENTED_EDGE('',*,*,#4169,.F.);
#5329=ORIENTED_EDGE('',*,*,#4170,.T.);
#5330=ORIENTED_EDGE('',*,*,#4171,.F.);
#5331=ORIENTED_EDGE('',*,*,#4167,.F.);
#5332=ORIENTED_EDGE('',*,*,#4172,.F.);
#5333=ORIENTED_EDGE('',*,*,#4173,.T.);
#5334=ORIENTED_EDGE('',*,*,#4174,.F.);
#5335=ORIENTED_EDGE('',*,*,#4170,.F.);
#5336=ORIENTED_EDGE('',*,*,#4175,.F.);
#5337=ORIENTED_EDGE('',*,*,#4176,.T.);
#5338=ORIENTED_EDGE('',*,*,#4177,.F.);
#5339=ORIENTED_EDGE('',*,*,#4173,.F.);
#5340=ORIENTED_EDGE('',*,*,#4178,.F.);
#5341=ORIENTED_EDGE('',*,*,#4179,.T.);
#5342=ORIENTED_EDGE('',*,*,#4180,.F.);
#5343=ORIENTED_EDGE('',*,*,#4176,.F.);
#5344=ORIENTED_EDGE('',*,*,#4181,.F.);
#5345=ORIENTED_EDGE('',*,*,#4182,.T.);
#5346=ORIENTED_EDGE('',*,*,#4183,.F.);
#5347=ORIENTED_EDGE('',*,*,#4179,.F.);
#5348=ORIENTED_EDGE('',*,*,#4184,.F.);
#5349=ORIENTED_EDGE('',*,*,#4185,.F.);
#5350=ORIENTED_EDGE('',*,*,#4186,.F.);
#5351=ORIENTED_EDGE('',*,*,#4182,.F.);
#5352=ORIENTED_EDGE('',*,*,#4187,.F.);
#5353=ORIENTED_EDGE('',*,*,#4188,.T.);
#5354=ORIENTED_EDGE('',*,*,#4189,.F.);
#5355=ORIENTED_EDGE('',*,*,#4190,.F.);
#5356=ORIENTED_EDGE('',*,*,#4191,.F.);
#5357=ORIENTED_EDGE('',*,*,#4192,.T.);
#5358=ORIENTED_EDGE('',*,*,#4193,.F.);
#5359=ORIENTED_EDGE('',*,*,#4188,.F.);
#5360=ORIENTED_EDGE('',*,*,#4194,.F.);
#5361=ORIENTED_EDGE('',*,*,#4195,.T.);
#5362=ORIENTED_EDGE('',*,*,#4196,.F.);
#5363=ORIENTED_EDGE('',*,*,#4192,.F.);
#5364=ORIENTED_EDGE('',*,*,#4197,.F.);
#5365=ORIENTED_EDGE('',*,*,#4198,.T.);
#5366=ORIENTED_EDGE('',*,*,#4199,.F.);
#5367=ORIENTED_EDGE('',*,*,#4195,.F.);
#5368=ORIENTED_EDGE('',*,*,#4200,.F.);
#5369=ORIENTED_EDGE('',*,*,#4201,.T.);
#5370=ORIENTED_EDGE('',*,*,#4202,.F.);
#5371=ORIENTED_EDGE('',*,*,#4198,.F.);
#5372=ORIENTED_EDGE('',*,*,#4203,.F.);
#5373=ORIENTED_EDGE('',*,*,#4204,.T.);
#5374=ORIENTED_EDGE('',*,*,#4205,.F.);
#5375=ORIENTED_EDGE('',*,*,#4201,.F.);
#5376=ORIENTED_EDGE('',*,*,#4206,.F.);
#5377=ORIENTED_EDGE('',*,*,#4207,.T.);
#5378=ORIENTED_EDGE('',*,*,#4208,.F.);
#5379=ORIENTED_EDGE('',*,*,#4204,.F.);
#5380=ORIENTED_EDGE('',*,*,#4209,.F.);
#5381=ORIENTED_EDGE('',*,*,#4210,.T.);
#5382=ORIENTED_EDGE('',*,*,#4211,.F.);
#5383=ORIENTED_EDGE('',*,*,#4207,.F.);
#5384=ORIENTED_EDGE('',*,*,#4212,.F.);
#5385=ORIENTED_EDGE('',*,*,#4213,.F.);
#5386=ORIENTED_EDGE('',*,*,#4214,.F.);
#5387=ORIENTED_EDGE('',*,*,#4210,.F.);
#5388=ORIENTED_EDGE('',*,*,#4215,.F.);
#5389=ORIENTED_EDGE('',*,*,#4216,.T.);
#5390=ORIENTED_EDGE('',*,*,#4217,.F.);
#5391=ORIENTED_EDGE('',*,*,#4218,.F.);
#5392=ORIENTED_EDGE('',*,*,#4219,.F.);
#5393=ORIENTED_EDGE('',*,*,#4220,.T.);
#5394=ORIENTED_EDGE('',*,*,#4221,.F.);
#5395=ORIENTED_EDGE('',*,*,#4216,.F.);
#5396=ORIENTED_EDGE('',*,*,#4222,.F.);
#5397=ORIENTED_EDGE('',*,*,#4223,.T.);
#5398=ORIENTED_EDGE('',*,*,#4224,.F.);
#5399=ORIENTED_EDGE('',*,*,#4220,.F.);
#5400=ORIENTED_EDGE('',*,*,#4225,.F.);
#5401=ORIENTED_EDGE('',*,*,#4226,.T.);
#5402=ORIENTED_EDGE('',*,*,#4227,.F.);
#5403=ORIENTED_EDGE('',*,*,#4223,.F.);
#5404=ORIENTED_EDGE('',*,*,#4228,.F.);
#5405=ORIENTED_EDGE('',*,*,#4229,.T.);
#5406=ORIENTED_EDGE('',*,*,#4230,.F.);
#5407=ORIENTED_EDGE('',*,*,#4226,.F.);
#5408=ORIENTED_EDGE('',*,*,#4231,.F.);
#5409=ORIENTED_EDGE('',*,*,#4232,.T.);
#5410=ORIENTED_EDGE('',*,*,#4233,.F.);
#5411=ORIENTED_EDGE('',*,*,#4229,.F.);
#5412=ORIENTED_EDGE('',*,*,#4234,.F.);
#5413=ORIENTED_EDGE('',*,*,#4235,.T.);
#5414=ORIENTED_EDGE('',*,*,#4236,.F.);
#5415=ORIENTED_EDGE('',*,*,#4232,.F.);
#5416=ORIENTED_EDGE('',*,*,#4237,.F.);
#5417=ORIENTED_EDGE('',*,*,#4238,.T.);
#5418=ORIENTED_EDGE('',*,*,#4239,.F.);
#5419=ORIENTED_EDGE('',*,*,#4235,.F.);
#5420=ORIENTED_EDGE('',*,*,#4240,.F.);
#5421=ORIENTED_EDGE('',*,*,#4241,.F.);
#5422=ORIENTED_EDGE('',*,*,#4242,.F.);
#5423=ORIENTED_EDGE('',*,*,#4238,.F.);
#5424=ORIENTED_EDGE('',*,*,#4243,.F.);
#5425=ORIENTED_EDGE('',*,*,#4244,.T.);
#5426=ORIENTED_EDGE('',*,*,#4245,.F.);
#5427=ORIENTED_EDGE('',*,*,#4246,.F.);
#5428=ORIENTED_EDGE('',*,*,#4247,.F.);
#5429=ORIENTED_EDGE('',*,*,#4248,.T.);
#5430=ORIENTED_EDGE('',*,*,#4249,.F.);
#5431=ORIENTED_EDGE('',*,*,#4244,.F.);
#5432=ORIENTED_EDGE('',*,*,#4250,.F.);
#5433=ORIENTED_EDGE('',*,*,#4251,.T.);
#5434=ORIENTED_EDGE('',*,*,#4252,.F.);
#5435=ORIENTED_EDGE('',*,*,#4248,.F.);
#5436=ORIENTED_EDGE('',*,*,#4253,.F.);
#5437=ORIENTED_EDGE('',*,*,#4254,.T.);
#5438=ORIENTED_EDGE('',*,*,#4255,.F.);
#5439=ORIENTED_EDGE('',*,*,#4251,.F.);
#5440=ORIENTED_EDGE('',*,*,#4256,.F.);
#5441=ORIENTED_EDGE('',*,*,#4257,.T.);
#5442=ORIENTED_EDGE('',*,*,#4258,.F.);
#5443=ORIENTED_EDGE('',*,*,#4254,.F.);
#5444=ORIENTED_EDGE('',*,*,#4259,.F.);
#5445=ORIENTED_EDGE('',*,*,#4260,.T.);
#5446=ORIENTED_EDGE('',*,*,#4261,.F.);
#5447=ORIENTED_EDGE('',*,*,#4257,.F.);
#5448=ORIENTED_EDGE('',*,*,#4262,.F.);
#5449=ORIENTED_EDGE('',*,*,#4263,.T.);
#5450=ORIENTED_EDGE('',*,*,#4264,.F.);
#5451=ORIENTED_EDGE('',*,*,#4260,.F.);
#5452=ORIENTED_EDGE('',*,*,#4265,.F.);
#5453=ORIENTED_EDGE('',*,*,#4266,.T.);
#5454=ORIENTED_EDGE('',*,*,#4267,.F.);
#5455=ORIENTED_EDGE('',*,*,#4263,.F.);
#5456=ORIENTED_EDGE('',*,*,#4268,.F.);
#5457=ORIENTED_EDGE('',*,*,#4269,.F.);
#5458=ORIENTED_EDGE('',*,*,#4270,.F.);
#5459=ORIENTED_EDGE('',*,*,#4266,.F.);
#5460=ORIENTED_EDGE('',*,*,#4271,.F.);
#5461=ORIENTED_EDGE('',*,*,#4272,.T.);
#5462=ORIENTED_EDGE('',*,*,#4273,.F.);
#5463=ORIENTED_EDGE('',*,*,#4272,.F.);
#5464=ORIENTED_EDGE('',*,*,#4185,.T.);
#5465=ORIENTED_EDGE('',*,*,#4274,.T.);
#5466=ORIENTED_EDGE('',*,*,#4275,.T.);
#5467=ORIENTED_EDGE('',*,*,#4276,.F.);
#5468=ORIENTED_EDGE('',*,*,#4162,.T.);
#5469=ORIENTED_EDGE('',*,*,#4277,.F.);
#5470=ORIENTED_EDGE('',*,*,#4278,.F.);
#5471=ORIENTED_EDGE('',*,*,#4279,.T.);
#5472=ORIENTED_EDGE('',*,*,#4213,.T.);
#5473=ORIENTED_EDGE('',*,*,#4280,.T.);
#5474=ORIENTED_EDGE('',*,*,#4278,.T.);
#5475=ORIENTED_EDGE('',*,*,#4281,.F.);
#5476=ORIENTED_EDGE('',*,*,#4190,.T.);
#5477=ORIENTED_EDGE('',*,*,#4282,.F.);
#5478=ORIENTED_EDGE('',*,*,#4283,.F.);
#5479=ORIENTED_EDGE('',*,*,#4284,.T.);
#5480=ORIENTED_EDGE('',*,*,#4241,.T.);
#5481=ORIENTED_EDGE('',*,*,#4285,.T.);
#5482=ORIENTED_EDGE('',*,*,#4283,.T.);
#5483=ORIENTED_EDGE('',*,*,#4286,.F.);
#5484=ORIENTED_EDGE('',*,*,#4218,.T.);
#5485=ORIENTED_EDGE('',*,*,#4287,.F.);
#5486=ORIENTED_EDGE('',*,*,#4288,.F.);
#5487=ORIENTED_EDGE('',*,*,#4289,.T.);
#5488=ORIENTED_EDGE('',*,*,#4269,.T.);
#5489=ORIENTED_EDGE('',*,*,#4290,.T.);
#5490=ORIENTED_EDGE('',*,*,#4288,.T.);
#5491=ORIENTED_EDGE('',*,*,#4291,.F.);
#5492=ORIENTED_EDGE('',*,*,#4246,.T.);
#5493=ORIENTED_EDGE('',*,*,#4292,.F.);
#5494=ORIENTED_EDGE('',*,*,#4275,.F.);
#5495=ORIENTED_EDGE('',*,*,#4293,.T.);
#5496=ORIENTED_EDGE('',*,*,#4161,.T.);
#5497=ORIENTED_EDGE('',*,*,#4165,.T.);
#5498=ORIENTED_EDGE('',*,*,#4168,.T.);
#5499=ORIENTED_EDGE('',*,*,#4171,.T.);
#5500=ORIENTED_EDGE('',*,*,#4174,.T.);
#5501=ORIENTED_EDGE('',*,*,#4177,.T.);
#5502=ORIENTED_EDGE('',*,*,#4180,.T.);
#5503=ORIENTED_EDGE('',*,*,#4183,.T.);
#5504=ORIENTED_EDGE('',*,*,#4186,.T.);
#5505=ORIENTED_EDGE('',*,*,#4276,.T.);
#5506=ORIENTED_EDGE('',*,*,#4292,.T.);
#5507=ORIENTED_EDGE('',*,*,#4245,.T.);
#5508=ORIENTED_EDGE('',*,*,#4249,.T.);
#5509=ORIENTED_EDGE('',*,*,#4252,.T.);
#5510=ORIENTED_EDGE('',*,*,#4255,.T.);
#5511=ORIENTED_EDGE('',*,*,#4258,.T.);
#5512=ORIENTED_EDGE('',*,*,#4261,.T.);
#5513=ORIENTED_EDGE('',*,*,#4264,.T.);
#5514=ORIENTED_EDGE('',*,*,#4267,.T.);
#5515=ORIENTED_EDGE('',*,*,#4270,.T.);
#5516=ORIENTED_EDGE('',*,*,#4291,.T.);
#5517=ORIENTED_EDGE('',*,*,#4287,.T.);
#5518=ORIENTED_EDGE('',*,*,#4217,.T.);
#5519=ORIENTED_EDGE('',*,*,#4221,.T.);
#5520=ORIENTED_EDGE('',*,*,#4224,.T.);
#5521=ORIENTED_EDGE('',*,*,#4227,.T.);
#5522=ORIENTED_EDGE('',*,*,#4230,.T.);
#5523=ORIENTED_EDGE('',*,*,#4233,.T.);
#5524=ORIENTED_EDGE('',*,*,#4236,.T.);
#5525=ORIENTED_EDGE('',*,*,#4239,.T.);
#5526=ORIENTED_EDGE('',*,*,#4242,.T.);
#5527=ORIENTED_EDGE('',*,*,#4286,.T.);
#5528=ORIENTED_EDGE('',*,*,#4282,.T.);
#5529=ORIENTED_EDGE('',*,*,#4189,.T.);
#5530=ORIENTED_EDGE('',*,*,#4193,.T.);
#5531=ORIENTED_EDGE('',*,*,#4196,.T.);
#5532=ORIENTED_EDGE('',*,*,#4199,.T.);
#5533=ORIENTED_EDGE('',*,*,#4202,.T.);
#5534=ORIENTED_EDGE('',*,*,#4205,.T.);
#5535=ORIENTED_EDGE('',*,*,#4208,.T.);
#5536=ORIENTED_EDGE('',*,*,#4211,.T.);
#5537=ORIENTED_EDGE('',*,*,#4214,.T.);
#5538=ORIENTED_EDGE('',*,*,#4281,.T.);
#5539=ORIENTED_EDGE('',*,*,#4277,.T.);
#5540=ORIENTED_EDGE('',*,*,#4273,.T.);
#5541=ORIENTED_EDGE('',*,*,#4159,.T.);
#5542=ORIENTED_EDGE('',*,*,#4279,.F.);
#5543=ORIENTED_EDGE('',*,*,#4280,.F.);
#5544=ORIENTED_EDGE('',*,*,#4212,.T.);
#5545=ORIENTED_EDGE('',*,*,#4209,.T.);
#5546=ORIENTED_EDGE('',*,*,#4206,.T.);
#5547=ORIENTED_EDGE('',*,*,#4203,.T.);
#5548=ORIENTED_EDGE('',*,*,#4200,.T.);
#5549=ORIENTED_EDGE('',*,*,#4197,.T.);
#5550=ORIENTED_EDGE('',*,*,#4194,.T.);
#5551=ORIENTED_EDGE('',*,*,#4191,.T.);
#5552=ORIENTED_EDGE('',*,*,#4187,.T.);
#5553=ORIENTED_EDGE('',*,*,#4284,.F.);
#5554=ORIENTED_EDGE('',*,*,#4285,.F.);
#5555=ORIENTED_EDGE('',*,*,#4240,.T.);
#5556=ORIENTED_EDGE('',*,*,#4237,.T.);
#5557=ORIENTED_EDGE('',*,*,#4234,.T.);
#5558=ORIENTED_EDGE('',*,*,#4231,.T.);
#5559=ORIENTED_EDGE('',*,*,#4228,.T.);
#5560=ORIENTED_EDGE('',*,*,#4225,.T.);
#5561=ORIENTED_EDGE('',*,*,#4222,.T.);
#5562=ORIENTED_EDGE('',*,*,#4219,.T.);
#5563=ORIENTED_EDGE('',*,*,#4215,.T.);
#5564=ORIENTED_EDGE('',*,*,#4289,.F.);
#5565=ORIENTED_EDGE('',*,*,#4290,.F.);
#5566=ORIENTED_EDGE('',*,*,#4268,.T.);
#5567=ORIENTED_EDGE('',*,*,#4265,.T.);
#5568=ORIENTED_EDGE('',*,*,#4262,.T.);
#5569=ORIENTED_EDGE('',*,*,#4259,.T.);
#5570=ORIENTED_EDGE('',*,*,#4256,.T.);
#5571=ORIENTED_EDGE('',*,*,#4253,.T.);
#5572=ORIENTED_EDGE('',*,*,#4250,.T.);
#5573=ORIENTED_EDGE('',*,*,#4247,.T.);
#5574=ORIENTED_EDGE('',*,*,#4243,.T.);
#5575=ORIENTED_EDGE('',*,*,#4293,.F.);
#5576=ORIENTED_EDGE('',*,*,#4274,.F.);
#5577=ORIENTED_EDGE('',*,*,#4184,.T.);
#5578=ORIENTED_EDGE('',*,*,#4181,.T.);
#5579=ORIENTED_EDGE('',*,*,#4178,.T.);
#5580=ORIENTED_EDGE('',*,*,#4175,.T.);
#5581=ORIENTED_EDGE('',*,*,#4172,.T.);
#5582=ORIENTED_EDGE('',*,*,#4169,.T.);
#5583=ORIENTED_EDGE('',*,*,#4166,.T.);
#5584=ORIENTED_EDGE('',*,*,#4163,.T.);
#5585=ORIENTED_EDGE('',*,*,#4271,.T.);
#5586=ORIENTED_EDGE('',*,*,#4294,.F.);
#5587=ORIENTED_EDGE('',*,*,#4295,.T.);
#5588=ORIENTED_EDGE('',*,*,#4296,.F.);
#5589=ORIENTED_EDGE('',*,*,#4295,.F.);
#5590=ORIENTED_EDGE('',*,*,#4294,.T.);
#5591=ORIENTED_EDGE('',*,*,#4297,.F.);
#5592=ORIENTED_EDGE('',*,*,#4298,.F.);
#5593=ORIENTED_EDGE('',*,*,#4299,.T.);
#5594=ORIENTED_EDGE('',*,*,#4300,.F.);
#5595=ORIENTED_EDGE('',*,*,#4299,.F.);
#5596=ORIENTED_EDGE('',*,*,#4298,.T.);
#5597=ORIENTED_EDGE('',*,*,#4301,.F.);
#5598=ORIENTED_EDGE('',*,*,#4302,.F.);
#5599=ORIENTED_EDGE('',*,*,#4303,.T.);
#5600=ORIENTED_EDGE('',*,*,#4304,.F.);
#5601=ORIENTED_EDGE('',*,*,#4303,.F.);
#5602=ORIENTED_EDGE('',*,*,#4302,.T.);
#5603=ORIENTED_EDGE('',*,*,#4305,.F.);
#5604=ORIENTED_EDGE('',*,*,#4306,.F.);
#5605=ORIENTED_EDGE('',*,*,#4307,.T.);
#5606=ORIENTED_EDGE('',*,*,#4308,.F.);
#5607=ORIENTED_EDGE('',*,*,#4307,.F.);
#5608=ORIENTED_EDGE('',*,*,#4306,.T.);
#5609=ORIENTED_EDGE('',*,*,#4309,.F.);
#5610=ORIENTED_EDGE('',*,*,#4310,.F.);
#5611=ORIENTED_EDGE('',*,*,#4311,.T.);
#5612=ORIENTED_EDGE('',*,*,#4297,.T.);
#5613=ORIENTED_EDGE('',*,*,#4311,.F.);
#5614=ORIENTED_EDGE('',*,*,#4312,.F.);
#5615=ORIENTED_EDGE('',*,*,#4313,.T.);
#5616=ORIENTED_EDGE('',*,*,#4301,.T.);
#5617=ORIENTED_EDGE('',*,*,#4313,.F.);
#5618=ORIENTED_EDGE('',*,*,#4314,.F.);
#5619=ORIENTED_EDGE('',*,*,#4315,.T.);
#5620=ORIENTED_EDGE('',*,*,#4305,.T.);
#5621=ORIENTED_EDGE('',*,*,#4315,.F.);
#5622=ORIENTED_EDGE('',*,*,#4316,.F.);
#5623=ORIENTED_EDGE('',*,*,#4317,.T.);
#5624=ORIENTED_EDGE('',*,*,#4309,.T.);
#5625=ORIENTED_EDGE('',*,*,#4317,.F.);
#5626=ORIENTED_EDGE('',*,*,#4318,.T.);
#5627=ORIENTED_EDGE('',*,*,#4319,.T.);
#5628=ORIENTED_EDGE('',*,*,#4320,.F.);
#5629=ORIENTED_EDGE('',*,*,#4321,.F.);
#5630=ORIENTED_EDGE('',*,*,#4322,.T.);
#5631=ORIENTED_EDGE('',*,*,#4321,.T.);
#5632=ORIENTED_EDGE('',*,*,#4323,.F.);
#5633=ORIENTED_EDGE('',*,*,#4324,.F.);
#5634=ORIENTED_EDGE('',*,*,#4325,.T.);
#5635=ORIENTED_EDGE('',*,*,#4324,.T.);
#5636=ORIENTED_EDGE('',*,*,#4326,.F.);
#5637=ORIENTED_EDGE('',*,*,#4327,.F.);
#5638=ORIENTED_EDGE('',*,*,#4328,.T.);
#5639=ORIENTED_EDGE('',*,*,#4327,.T.);
#5640=ORIENTED_EDGE('',*,*,#4329,.F.);
#5641=ORIENTED_EDGE('',*,*,#4330,.F.);
#5642=ORIENTED_EDGE('',*,*,#4331,.T.);
#5643=ORIENTED_EDGE('',*,*,#4330,.T.);
#5644=ORIENTED_EDGE('',*,*,#4332,.F.);
#5645=ORIENTED_EDGE('',*,*,#4333,.F.);
#5646=ORIENTED_EDGE('',*,*,#4308,.T.);
#5647=ORIENTED_EDGE('',*,*,#4304,.T.);
#5648=ORIENTED_EDGE('',*,*,#4300,.T.);
#5649=ORIENTED_EDGE('',*,*,#4296,.T.);
#5650=ORIENTED_EDGE('',*,*,#4334,.T.);
#5651=ORIENTED_EDGE('',*,*,#4333,.T.);
#5652=ORIENTED_EDGE('',*,*,#4335,.F.);
#5653=ORIENTED_EDGE('',*,*,#4336,.F.);
#5654=ORIENTED_EDGE('',*,*,#4337,.T.);
#5655=ORIENTED_EDGE('',*,*,#4336,.T.);
#5656=ORIENTED_EDGE('',*,*,#4338,.F.);
#5657=ORIENTED_EDGE('',*,*,#4339,.F.);
#5658=ORIENTED_EDGE('',*,*,#4340,.T.);
#5659=ORIENTED_EDGE('',*,*,#4339,.T.);
#5660=ORIENTED_EDGE('',*,*,#4341,.F.);
#5661=ORIENTED_EDGE('',*,*,#4342,.F.);
#5662=ORIENTED_EDGE('',*,*,#4343,.T.);
#5663=ORIENTED_EDGE('',*,*,#4342,.T.);
#5664=ORIENTED_EDGE('',*,*,#4344,.F.);
#5665=ORIENTED_EDGE('',*,*,#4345,.F.);
#5666=ORIENTED_EDGE('',*,*,#4346,.T.);
#5667=ORIENTED_EDGE('',*,*,#4345,.T.);
#5668=ORIENTED_EDGE('',*,*,#4347,.F.);
#5669=ORIENTED_EDGE('',*,*,#4348,.F.);
#5670=ORIENTED_EDGE('',*,*,#4349,.T.);
#5671=ORIENTED_EDGE('',*,*,#4348,.T.);
#5672=ORIENTED_EDGE('',*,*,#4350,.F.);
#5673=ORIENTED_EDGE('',*,*,#4351,.F.);
#5674=ORIENTED_EDGE('',*,*,#4310,.T.);
#5675=ORIENTED_EDGE('',*,*,#4312,.T.);
#5676=ORIENTED_EDGE('',*,*,#4314,.T.);
#5677=ORIENTED_EDGE('',*,*,#4316,.T.);
#5678=ORIENTED_EDGE('',*,*,#4352,.T.);
#5679=ORIENTED_EDGE('',*,*,#4351,.T.);
#5680=ORIENTED_EDGE('',*,*,#4353,.F.);
#5681=ORIENTED_EDGE('',*,*,#4319,.F.);
#5682=ORIENTED_EDGE('',*,*,#4353,.T.);
#5683=ORIENTED_EDGE('',*,*,#4350,.T.);
#5684=ORIENTED_EDGE('',*,*,#4347,.T.);
#5685=ORIENTED_EDGE('',*,*,#4344,.T.);
#5686=ORIENTED_EDGE('',*,*,#4341,.T.);
#5687=ORIENTED_EDGE('',*,*,#4338,.T.);
#5688=ORIENTED_EDGE('',*,*,#4335,.T.);
#5689=ORIENTED_EDGE('',*,*,#4332,.T.);
#5690=ORIENTED_EDGE('',*,*,#4329,.T.);
#5691=ORIENTED_EDGE('',*,*,#4326,.T.);
#5692=ORIENTED_EDGE('',*,*,#4323,.T.);
#5693=ORIENTED_EDGE('',*,*,#4320,.T.);
#5694=ORIENTED_EDGE('',*,*,#4352,.F.);
#5695=ORIENTED_EDGE('',*,*,#4318,.F.);
#5696=ORIENTED_EDGE('',*,*,#4322,.F.);
#5697=ORIENTED_EDGE('',*,*,#4325,.F.);
#5698=ORIENTED_EDGE('',*,*,#4328,.F.);
#5699=ORIENTED_EDGE('',*,*,#4331,.F.);
#5700=ORIENTED_EDGE('',*,*,#4334,.F.);
#5701=ORIENTED_EDGE('',*,*,#4337,.F.);
#5702=ORIENTED_EDGE('',*,*,#4340,.F.);
#5703=ORIENTED_EDGE('',*,*,#4343,.F.);
#5704=ORIENTED_EDGE('',*,*,#4346,.F.);
#5705=ORIENTED_EDGE('',*,*,#4349,.F.);
#5706=ORIENTED_EDGE('',*,*,#4354,.T.);
#5707=ORIENTED_EDGE('',*,*,#4355,.T.);
#5708=ORIENTED_EDGE('',*,*,#4356,.T.);
#5709=ORIENTED_EDGE('',*,*,#4357,.F.);
#5710=ORIENTED_EDGE('',*,*,#4358,.T.);
#5711=ORIENTED_EDGE('',*,*,#4359,.T.);
#5712=ORIENTED_EDGE('',*,*,#4360,.T.);
#5713=ORIENTED_EDGE('',*,*,#4355,.F.);
#5714=ORIENTED_EDGE('',*,*,#4361,.T.);
#5715=ORIENTED_EDGE('',*,*,#4362,.T.);
#5716=ORIENTED_EDGE('',*,*,#4363,.T.);
#5717=ORIENTED_EDGE('',*,*,#4359,.F.);
#5718=ORIENTED_EDGE('',*,*,#4364,.T.);
#5719=ORIENTED_EDGE('',*,*,#4365,.T.);
#5720=ORIENTED_EDGE('',*,*,#4366,.T.);
#5721=ORIENTED_EDGE('',*,*,#4362,.F.);
#5722=ORIENTED_EDGE('',*,*,#4367,.T.);
#5723=ORIENTED_EDGE('',*,*,#4368,.T.);
#5724=ORIENTED_EDGE('',*,*,#4369,.T.);
#5725=ORIENTED_EDGE('',*,*,#4365,.F.);
#5726=ORIENTED_EDGE('',*,*,#4370,.T.);
#5727=ORIENTED_EDGE('',*,*,#4357,.T.);
#5728=ORIENTED_EDGE('',*,*,#4371,.T.);
#5729=ORIENTED_EDGE('',*,*,#4368,.F.);
#5730=ORIENTED_EDGE('',*,*,#4370,.F.);
#5731=ORIENTED_EDGE('',*,*,#4367,.F.);
#5732=ORIENTED_EDGE('',*,*,#4364,.F.);
#5733=ORIENTED_EDGE('',*,*,#4361,.F.);
#5734=ORIENTED_EDGE('',*,*,#4358,.F.);
#5735=ORIENTED_EDGE('',*,*,#4354,.F.);
#5736=ORIENTED_EDGE('',*,*,#4371,.F.);
#5737=ORIENTED_EDGE('',*,*,#4356,.F.);
#5738=ORIENTED_EDGE('',*,*,#4360,.F.);
#5739=ORIENTED_EDGE('',*,*,#4363,.F.);
#5740=ORIENTED_EDGE('',*,*,#4366,.F.);
#5741=ORIENTED_EDGE('',*,*,#4369,.F.);
#5742=ORIENTED_EDGE('',*,*,#4372,.T.);
#5743=ORIENTED_EDGE('',*,*,#4373,.F.);
#5744=ORIENTED_EDGE('',*,*,#4372,.F.);
#5745=ORIENTED_EDGE('',*,*,#4374,.T.);
#5746=ORIENTED_EDGE('',*,*,#4375,.T.);
#5747=ORIENTED_EDGE('',*,*,#4374,.F.);
#5748=ORIENTED_EDGE('',*,*,#4375,.F.);
#5749=ORIENTED_EDGE('',*,*,#4376,.F.);
#5750=ORIENTED_EDGE('',*,*,#4377,.F.);
#5751=ORIENTED_EDGE('',*,*,#4378,.T.);
#5752=ORIENTED_EDGE('',*,*,#4376,.T.);
#5753=ORIENTED_EDGE('',*,*,#4378,.F.);
#5754=ORIENTED_EDGE('',*,*,#4379,.F.);
#5755=ORIENTED_EDGE('',*,*,#4380,.T.);
#5756=ORIENTED_EDGE('',*,*,#4377,.T.);
#5757=ORIENTED_EDGE('',*,*,#4380,.F.);
#5758=ORIENTED_EDGE('',*,*,#4381,.F.);
#5759=ORIENTED_EDGE('',*,*,#4382,.T.);
#5760=ORIENTED_EDGE('',*,*,#4379,.T.);
#5761=ORIENTED_EDGE('',*,*,#4382,.F.);
#5762=ORIENTED_EDGE('',*,*,#4381,.T.);
#5763=ORIENTED_EDGE('',*,*,#4383,.F.);
#5764=ORIENTED_EDGE('',*,*,#4384,.F.);
#5765=ORIENTED_EDGE('',*,*,#4385,.T.);
#5766=ORIENTED_EDGE('',*,*,#4383,.T.);
#5767=ORIENTED_EDGE('',*,*,#4385,.F.);
#5768=ORIENTED_EDGE('',*,*,#4373,.T.);
#5769=ORIENTED_EDGE('',*,*,#4386,.T.);
#5770=ORIENTED_EDGE('',*,*,#4384,.T.);
#5771=ORIENTED_EDGE('',*,*,#4386,.F.);
#5772=ORIENTED_EDGE('',*,*,#4387,.F.);
#5773=ORIENTED_EDGE('',*,*,#4388,.F.);
#5774=ORIENTED_EDGE('',*,*,#4389,.T.);
#5775=ORIENTED_EDGE('',*,*,#4387,.T.);
#5776=ORIENTED_EDGE('',*,*,#4389,.F.);
#5777=ORIENTED_EDGE('',*,*,#4390,.F.);
#5778=ORIENTED_EDGE('',*,*,#4391,.T.);
#5779=ORIENTED_EDGE('',*,*,#4388,.T.);
#5780=ORIENTED_EDGE('',*,*,#4391,.F.);
#5781=ORIENTED_EDGE('',*,*,#4392,.F.);
#5782=ORIENTED_EDGE('',*,*,#4393,.T.);
#5783=ORIENTED_EDGE('',*,*,#4390,.T.);
#5784=ORIENTED_EDGE('',*,*,#4393,.F.);
#5785=ORIENTED_EDGE('',*,*,#4392,.T.);
#5786=ORIENTED_EDGE('',*,*,#4394,.F.);
#5787=ORIENTED_EDGE('',*,*,#4395,.F.);
#5788=ORIENTED_EDGE('',*,*,#4396,.T.);
#5789=ORIENTED_EDGE('',*,*,#4394,.T.);
#5790=ORIENTED_EDGE('',*,*,#4396,.F.);
#5791=ORIENTED_EDGE('',*,*,#4397,.F.);
#5792=ORIENTED_EDGE('',*,*,#4398,.T.);
#5793=ORIENTED_EDGE('',*,*,#4395,.T.);
#5794=ORIENTED_EDGE('',*,*,#4398,.F.);
#5795=ORIENTED_EDGE('',*,*,#4399,.F.);
#5796=ORIENTED_EDGE('',*,*,#4400,.T.);
#5797=ORIENTED_EDGE('',*,*,#4397,.T.);
#5798=ORIENTED_EDGE('',*,*,#4400,.F.);
#5799=ORIENTED_EDGE('',*,*,#4399,.T.);
#5800=ORIENTED_EDGE('',*,*,#4401,.T.);
#5801=ORIENTED_EDGE('',*,*,#4402,.T.);
#5802=ORIENTED_EDGE('',*,*,#4403,.T.);
#5803=ORIENTED_EDGE('',*,*,#4404,.F.);
#5804=ORIENTED_EDGE('',*,*,#4405,.T.);
#5805=ORIENTED_EDGE('',*,*,#4406,.T.);
#5806=ORIENTED_EDGE('',*,*,#4407,.T.);
#5807=ORIENTED_EDGE('',*,*,#4402,.F.);
#5808=ORIENTED_EDGE('',*,*,#4408,.T.);
#5809=ORIENTED_EDGE('',*,*,#4409,.T.);
#5810=ORIENTED_EDGE('',*,*,#4410,.T.);
#5811=ORIENTED_EDGE('',*,*,#4406,.F.);
#5812=ORIENTED_EDGE('',*,*,#4411,.T.);
#5813=ORIENTED_EDGE('',*,*,#4412,.T.);
#5814=ORIENTED_EDGE('',*,*,#4413,.T.);
#5815=ORIENTED_EDGE('',*,*,#4409,.F.);
#5816=ORIENTED_EDGE('',*,*,#4414,.T.);
#5817=ORIENTED_EDGE('',*,*,#4415,.T.);
#5818=ORIENTED_EDGE('',*,*,#4416,.T.);
#5819=ORIENTED_EDGE('',*,*,#4412,.F.);
#5820=ORIENTED_EDGE('',*,*,#4417,.T.);
#5821=ORIENTED_EDGE('',*,*,#4404,.T.);
#5822=ORIENTED_EDGE('',*,*,#4418,.T.);
#5823=ORIENTED_EDGE('',*,*,#4415,.F.);
#5824=ORIENTED_EDGE('',*,*,#4417,.F.);
#5825=ORIENTED_EDGE('',*,*,#4414,.F.);
#5826=ORIENTED_EDGE('',*,*,#4411,.F.);
#5827=ORIENTED_EDGE('',*,*,#4408,.F.);
#5828=ORIENTED_EDGE('',*,*,#4405,.F.);
#5829=ORIENTED_EDGE('',*,*,#4401,.F.);
#5830=ORIENTED_EDGE('',*,*,#4418,.F.);
#5831=ORIENTED_EDGE('',*,*,#4403,.F.);
#5832=ORIENTED_EDGE('',*,*,#4407,.F.);
#5833=ORIENTED_EDGE('',*,*,#4410,.F.);
#5834=ORIENTED_EDGE('',*,*,#4413,.F.);
#5835=ORIENTED_EDGE('',*,*,#4416,.F.);
#5836=ORIENTED_EDGE('',*,*,#4419,.F.);
#5837=ORIENTED_EDGE('',*,*,#4420,.F.);
#5838=ORIENTED_EDGE('',*,*,#4421,.F.);
#5839=ORIENTED_EDGE('',*,*,#4422,.F.);
#5840=ORIENTED_EDGE('',*,*,#4421,.T.);
#5841=ORIENTED_EDGE('',*,*,#4423,.T.);
#5842=ORIENTED_EDGE('',*,*,#4424,.F.);
#5843=ORIENTED_EDGE('',*,*,#4425,.F.);
#5844=ORIENTED_EDGE('',*,*,#4426,.T.);
#5845=ORIENTED_EDGE('',*,*,#4427,.T.);
#5846=ORIENTED_EDGE('',*,*,#4428,.T.);
#5847=ORIENTED_EDGE('',*,*,#4424,.T.);
#5848=ORIENTED_EDGE('',*,*,#4429,.T.);
#5849=ORIENTED_EDGE('',*,*,#4426,.F.);
#5850=ORIENTED_EDGE('',*,*,#4423,.F.);
#5851=ORIENTED_EDGE('',*,*,#4420,.T.);
#5852=ORIENTED_EDGE('',*,*,#4430,.F.);
#5853=ORIENTED_EDGE('',*,*,#4431,.F.);
#5854=ORIENTED_EDGE('',*,*,#4432,.T.);
#5855=ORIENTED_EDGE('',*,*,#4433,.F.);
#5856=ORIENTED_EDGE('',*,*,#4434,.T.);
#5857=ORIENTED_EDGE('',*,*,#4435,.T.);
#5858=ORIENTED_EDGE('',*,*,#4436,.T.);
#5859=ORIENTED_EDGE('',*,*,#4437,.T.);
#5860=ORIENTED_EDGE('',*,*,#4438,.T.);
#5861=ORIENTED_EDGE('',*,*,#4427,.F.);
#5862=ORIENTED_EDGE('',*,*,#4436,.F.);
#5863=ORIENTED_EDGE('',*,*,#4439,.F.);
#5864=ORIENTED_EDGE('',*,*,#4440,.F.);
#5865=ORIENTED_EDGE('',*,*,#4437,.F.);
#5866=ORIENTED_EDGE('',*,*,#4435,.F.);
#5867=ORIENTED_EDGE('',*,*,#4428,.F.);
#5868=ORIENTED_EDGE('',*,*,#4438,.F.);
#5869=ORIENTED_EDGE('',*,*,#4440,.T.);
#5870=ORIENTED_EDGE('',*,*,#4441,.F.);
#5871=ORIENTED_EDGE('',*,*,#4442,.F.);
#5872=ORIENTED_EDGE('',*,*,#4443,.T.);
#5873=ORIENTED_EDGE('',*,*,#4444,.F.);
#5874=ORIENTED_EDGE('',*,*,#4445,.T.);
#5875=ORIENTED_EDGE('',*,*,#4422,.T.);
#5876=ORIENTED_EDGE('',*,*,#4425,.T.);
#5877=ORIENTED_EDGE('',*,*,#4439,.T.);
#5878=ORIENTED_EDGE('',*,*,#4434,.F.);
#5879=ORIENTED_EDGE('',*,*,#4446,.F.);
#5880=ORIENTED_EDGE('',*,*,#4441,.T.);
#5881=ORIENTED_EDGE('',*,*,#4442,.T.);
#5882=ORIENTED_EDGE('',*,*,#4446,.T.);
#5883=ORIENTED_EDGE('',*,*,#4433,.T.);
#5884=ORIENTED_EDGE('',*,*,#4447,.T.);
#5885=ORIENTED_EDGE('',*,*,#4448,.T.);
#5886=ORIENTED_EDGE('',*,*,#4449,.T.);
#5887=ORIENTED_EDGE('',*,*,#4448,.F.);
#5888=ORIENTED_EDGE('',*,*,#4450,.F.);
#5889=ORIENTED_EDGE('',*,*,#4451,.T.);
#5890=ORIENTED_EDGE('',*,*,#4429,.F.);
#5891=ORIENTED_EDGE('',*,*,#4451,.F.);
#5892=ORIENTED_EDGE('',*,*,#4452,.F.);
#5893=ORIENTED_EDGE('',*,*,#4453,.F.);
#5894=ORIENTED_EDGE('',*,*,#4454,.F.);
#5895=ORIENTED_EDGE('',*,*,#4447,.F.);
#5896=ORIENTED_EDGE('',*,*,#4432,.F.);
#5897=ORIENTED_EDGE('',*,*,#4455,.F.);
#5898=ORIENTED_EDGE('',*,*,#4452,.T.);
#5899=ORIENTED_EDGE('',*,*,#4450,.T.);
#5900=ORIENTED_EDGE('',*,*,#4449,.F.);
#5901=ORIENTED_EDGE('',*,*,#4454,.T.);
#5902=ORIENTED_EDGE('',*,*,#4456,.F.);
#5903=ORIENTED_EDGE('',*,*,#4443,.F.);
#5904=ORIENTED_EDGE('',*,*,#4431,.T.);
#5905=ORIENTED_EDGE('',*,*,#4457,.T.);
#5906=ORIENTED_EDGE('',*,*,#4444,.T.);
#5907=ORIENTED_EDGE('',*,*,#4456,.T.);
#5908=ORIENTED_EDGE('',*,*,#4453,.T.);
#5909=ORIENTED_EDGE('',*,*,#4455,.T.);
#5910=ORIENTED_EDGE('',*,*,#4419,.T.);
#5911=ORIENTED_EDGE('',*,*,#4445,.F.);
#5912=ORIENTED_EDGE('',*,*,#4457,.F.);
#5913=ORIENTED_EDGE('',*,*,#4430,.T.);
#5914=ORIENTED_EDGE('',*,*,#4458,.T.);
#5915=ORIENTED_EDGE('',*,*,#4459,.T.);
#5916=ORIENTED_EDGE('',*,*,#4460,.T.);
#5917=ORIENTED_EDGE('',*,*,#4459,.F.);
#5918=ORIENTED_EDGE('',*,*,#4460,.F.);
#5919=ORIENTED_EDGE('',*,*,#4461,.T.);
#5920=ORIENTED_EDGE('',*,*,#4462,.T.);
#5921=ORIENTED_EDGE('',*,*,#4461,.F.);
#5922=ORIENTED_EDGE('',*,*,#4463,.T.);
#5923=ORIENTED_EDGE('',*,*,#4458,.F.);
#5924=ORIENTED_EDGE('',*,*,#4463,.F.);
#5925=ORIENTED_EDGE('',*,*,#4464,.T.);
#5926=ORIENTED_EDGE('',*,*,#4465,.T.);
#5927=ORIENTED_EDGE('',*,*,#4464,.F.);
#5928=ORIENTED_EDGE('',*,*,#4465,.F.);
#5929=ORIENTED_EDGE('',*,*,#4462,.F.);
#5930=ORIENTED_EDGE('',*,*,#4466,.F.);
#5931=ORIENTED_EDGE('',*,*,#4467,.T.);
#5932=ORIENTED_EDGE('',*,*,#4468,.F.);
#5933=ORIENTED_EDGE('',*,*,#4467,.F.);
#5934=ORIENTED_EDGE('',*,*,#4469,.F.);
#5935=ORIENTED_EDGE('',*,*,#4470,.F.);
#5936=ORIENTED_EDGE('',*,*,#4471,.F.);
#5937=ORIENTED_EDGE('',*,*,#4472,.F.);
#5938=ORIENTED_EDGE('',*,*,#4471,.T.);
#5939=ORIENTED_EDGE('',*,*,#4473,.T.);
#5940=ORIENTED_EDGE('',*,*,#4474,.F.);
#5941=ORIENTED_EDGE('',*,*,#4475,.F.);
#5942=ORIENTED_EDGE('',*,*,#4476,.F.);
#5943=ORIENTED_EDGE('',*,*,#4477,.T.);
#5944=ORIENTED_EDGE('',*,*,#4474,.T.);
#5945=ORIENTED_EDGE('',*,*,#4478,.T.);
#5946=ORIENTED_EDGE('',*,*,#4469,.T.);
#5947=ORIENTED_EDGE('',*,*,#4479,.F.);
#5948=ORIENTED_EDGE('',*,*,#4480,.T.);
#5949=ORIENTED_EDGE('',*,*,#4481,.T.);
#5950=ORIENTED_EDGE('',*,*,#4476,.T.);
#5951=ORIENTED_EDGE('',*,*,#4482,.T.);
#5952=ORIENTED_EDGE('',*,*,#4483,.T.);
#5953=ORIENTED_EDGE('',*,*,#4484,.T.);
#5954=ORIENTED_EDGE('',*,*,#4485,.F.);
#5955=ORIENTED_EDGE('',*,*,#4486,.F.);
#5956=ORIENTED_EDGE('',*,*,#4487,.F.);
#5957=ORIENTED_EDGE('',*,*,#4488,.T.);
#5958=ORIENTED_EDGE('',*,*,#4489,.F.);
#5959=ORIENTED_EDGE('',*,*,#4488,.F.);
#5960=ORIENTED_EDGE('',*,*,#4490,.F.);
#5961=ORIENTED_EDGE('',*,*,#4491,.T.);
#5962=ORIENTED_EDGE('',*,*,#4492,.F.);
#5963=ORIENTED_EDGE('',*,*,#4491,.F.);
#5964=ORIENTED_EDGE('',*,*,#4493,.F.);
#5965=ORIENTED_EDGE('',*,*,#4494,.T.);
#5966=ORIENTED_EDGE('',*,*,#4495,.F.);
#5967=ORIENTED_EDGE('',*,*,#4494,.F.);
#5968=ORIENTED_EDGE('',*,*,#4496,.F.);
#5969=ORIENTED_EDGE('',*,*,#4497,.F.);
#5970=ORIENTED_EDGE('',*,*,#4498,.F.);
#5971=ORIENTED_EDGE('',*,*,#4499,.T.);
#5972=ORIENTED_EDGE('',*,*,#4500,.F.);
#5973=ORIENTED_EDGE('',*,*,#4497,.T.);
#5974=ORIENTED_EDGE('',*,*,#4481,.F.);
#5975=ORIENTED_EDGE('',*,*,#4501,.T.);
#5976=ORIENTED_EDGE('',*,*,#4502,.T.);
#5977=ORIENTED_EDGE('',*,*,#4503,.T.);
#5978=ORIENTED_EDGE('',*,*,#4504,.F.);
#5979=ORIENTED_EDGE('',*,*,#4505,.T.);
#5980=ORIENTED_EDGE('',*,*,#4499,.F.);
#5981=ORIENTED_EDGE('',*,*,#4506,.T.);
#5982=ORIENTED_EDGE('',*,*,#4482,.F.);
#5983=ORIENTED_EDGE('',*,*,#4478,.F.);
#5984=ORIENTED_EDGE('',*,*,#4473,.F.);
#5985=ORIENTED_EDGE('',*,*,#4470,.T.);
#5986=ORIENTED_EDGE('',*,*,#4466,.T.);
#5987=ORIENTED_EDGE('',*,*,#4507,.T.);
#5988=ORIENTED_EDGE('',*,*,#4508,.T.);
#5989=ORIENTED_EDGE('',*,*,#4509,.F.);
#5990=ORIENTED_EDGE('',*,*,#4510,.T.);
#5991=ORIENTED_EDGE('',*,*,#4507,.F.);
#5992=ORIENTED_EDGE('',*,*,#4511,.T.);
#5993=ORIENTED_EDGE('',*,*,#4512,.F.);
#5994=ORIENTED_EDGE('',*,*,#4511,.F.);
#5995=ORIENTED_EDGE('',*,*,#4496,.T.);
#5996=ORIENTED_EDGE('',*,*,#4505,.F.);
#5997=ORIENTED_EDGE('',*,*,#4513,.T.);
#5998=ORIENTED_EDGE('',*,*,#4514,.T.);
#5999=ORIENTED_EDGE('',*,*,#4515,.T.);
#6000=ORIENTED_EDGE('',*,*,#4503,.F.);
#6001=ORIENTED_EDGE('',*,*,#4516,.F.);
#6002=ORIENTED_EDGE('',*,*,#4517,.F.);
#6003=ORIENTED_EDGE('',*,*,#4518,.F.);
#6004=ORIENTED_EDGE('',*,*,#4519,.F.);
#6005=ORIENTED_EDGE('',*,*,#4520,.F.);
#6006=ORIENTED_EDGE('',*,*,#4506,.F.);
#6007=ORIENTED_EDGE('',*,*,#4498,.T.);
#6008=ORIENTED_EDGE('',*,*,#4500,.T.);
#6009=ORIENTED_EDGE('',*,*,#4487,.T.);
#6010=ORIENTED_EDGE('',*,*,#4490,.T.);
#6011=ORIENTED_EDGE('',*,*,#4493,.T.);
#6012=ORIENTED_EDGE('',*,*,#4510,.F.);
#6013=ORIENTED_EDGE('',*,*,#4521,.T.);
#6014=ORIENTED_EDGE('',*,*,#4522,.F.);
#6015=ORIENTED_EDGE('',*,*,#4521,.F.);
#6016=ORIENTED_EDGE('',*,*,#4515,.F.);
#6017=ORIENTED_EDGE('',*,*,#4523,.F.);
#6018=ORIENTED_EDGE('',*,*,#4513,.F.);
#6019=ORIENTED_EDGE('',*,*,#4504,.T.);
#6020=ORIENTED_EDGE('',*,*,#4514,.F.);
#6021=ORIENTED_EDGE('',*,*,#4523,.T.);
#6022=ORIENTED_EDGE('',*,*,#4509,.T.);
#6023=ORIENTED_EDGE('',*,*,#4524,.T.);
#6024=ORIENTED_EDGE('',*,*,#4525,.F.);
#6025=ORIENTED_EDGE('',*,*,#4524,.F.);
#6026=ORIENTED_EDGE('',*,*,#4508,.F.);
#6027=ORIENTED_EDGE('',*,*,#4526,.T.);
#6028=ORIENTED_EDGE('',*,*,#4527,.F.);
#6029=ORIENTED_EDGE('',*,*,#4526,.F.);
#6030=ORIENTED_EDGE('',*,*,#4528,.T.);
#6031=ORIENTED_EDGE('',*,*,#4529,.F.);
#6032=ORIENTED_EDGE('',*,*,#4530,.F.);
#6033=ORIENTED_EDGE('',*,*,#4516,.T.);
#6034=ORIENTED_EDGE('',*,*,#4483,.F.);
#6035=ORIENTED_EDGE('',*,*,#4520,.T.);
#6036=ORIENTED_EDGE('',*,*,#4531,.T.);
#6037=ORIENTED_EDGE('',*,*,#4532,.F.);
#6038=ORIENTED_EDGE('',*,*,#4519,.T.);
#6039=ORIENTED_EDGE('',*,*,#4533,.T.);
#6040=ORIENTED_EDGE('',*,*,#4534,.F.);
#6041=ORIENTED_EDGE('',*,*,#4531,.F.);
#6042=ORIENTED_EDGE('',*,*,#4517,.T.);
#6043=ORIENTED_EDGE('',*,*,#4530,.T.);
#6044=ORIENTED_EDGE('',*,*,#4535,.F.);
#6045=ORIENTED_EDGE('',*,*,#4536,.F.);
#6046=ORIENTED_EDGE('',*,*,#4518,.T.);
#6047=ORIENTED_EDGE('',*,*,#4536,.T.);
#6048=ORIENTED_EDGE('',*,*,#4537,.F.);
#6049=ORIENTED_EDGE('',*,*,#4533,.F.);
#6050=ORIENTED_EDGE('',*,*,#4537,.T.);
#6051=ORIENTED_EDGE('',*,*,#4535,.T.);
#6052=ORIENTED_EDGE('',*,*,#4529,.T.);
#6053=ORIENTED_EDGE('',*,*,#4538,.F.);
#6054=ORIENTED_EDGE('',*,*,#4532,.T.);
#6055=ORIENTED_EDGE('',*,*,#4534,.T.);
#6056=ORIENTED_EDGE('',*,*,#4489,.T.);
#6057=ORIENTED_EDGE('',*,*,#4492,.T.);
#6058=ORIENTED_EDGE('',*,*,#4495,.T.);
#6059=ORIENTED_EDGE('',*,*,#4538,.T.);
#6060=ORIENTED_EDGE('',*,*,#4539,.T.);
#6061=ORIENTED_EDGE('',*,*,#4540,.F.);
#6062=ORIENTED_EDGE('',*,*,#4484,.F.);
#6063=ORIENTED_EDGE('',*,*,#4486,.T.);
#6064=ORIENTED_EDGE('',*,*,#4541,.F.);
#6065=ORIENTED_EDGE('',*,*,#4542,.F.);
#6066=ORIENTED_EDGE('',*,*,#4543,.T.);
#6067=ORIENTED_EDGE('',*,*,#4479,.T.);
#6068=ORIENTED_EDGE('',*,*,#4472,.T.);
#6069=ORIENTED_EDGE('',*,*,#4475,.T.);
#6070=ORIENTED_EDGE('',*,*,#4477,.F.);
#6071=ORIENTED_EDGE('',*,*,#4468,.T.);
#6072=ORIENTED_EDGE('',*,*,#4512,.T.);
#6073=ORIENTED_EDGE('',*,*,#4522,.T.);
#6074=ORIENTED_EDGE('',*,*,#4525,.T.);
#6075=ORIENTED_EDGE('',*,*,#4527,.T.);
#6076=ORIENTED_EDGE('',*,*,#4544,.T.);
#6077=ORIENTED_EDGE('',*,*,#4542,.T.);
#6078=ORIENTED_EDGE('',*,*,#4545,.F.);
#6079=ORIENTED_EDGE('',*,*,#4539,.F.);
#6080=ORIENTED_EDGE('',*,*,#4528,.F.);
#6081=ORIENTED_EDGE('',*,*,#4502,.F.);
#6082=ORIENTED_EDGE('',*,*,#4540,.T.);
#6083=ORIENTED_EDGE('',*,*,#4545,.T.);
#6084=ORIENTED_EDGE('',*,*,#4541,.T.);
#6085=ORIENTED_EDGE('',*,*,#4485,.T.);
#6086=ORIENTED_EDGE('',*,*,#4501,.F.);
#6087=ORIENTED_EDGE('',*,*,#4480,.F.);
#6088=ORIENTED_EDGE('',*,*,#4543,.F.);
#6089=ORIENTED_EDGE('',*,*,#4544,.F.);
#6090=ORIENTED_EDGE('',*,*,#4546,.F.);
#6091=ORIENTED_EDGE('',*,*,#4547,.T.);
#6092=ORIENTED_EDGE('',*,*,#4548,.F.);
#6093=ORIENTED_EDGE('',*,*,#4547,.F.);
#6094=ORIENTED_EDGE('',*,*,#4549,.F.);
#6095=ORIENTED_EDGE('',*,*,#4550,.T.);
#6096=ORIENTED_EDGE('',*,*,#4551,.T.);
#6097=ORIENTED_EDGE('',*,*,#4550,.F.);
#6098=ORIENTED_EDGE('',*,*,#4549,.T.);
#6099=ORIENTED_EDGE('',*,*,#4548,.T.);
#6100=ORIENTED_EDGE('',*,*,#4551,.F.);
#6101=ORIENTED_EDGE('',*,*,#4546,.T.);
#6102=ORIENTED_EDGE('',*,*,#4552,.F.);
#6103=ORIENTED_EDGE('',*,*,#4553,.T.);
#6104=ORIENTED_EDGE('',*,*,#4554,.F.);
#6105=ORIENTED_EDGE('',*,*,#4553,.F.);
#6106=ORIENTED_EDGE('',*,*,#4552,.T.);
#6107=ORIENTED_EDGE('',*,*,#4555,.F.);
#6108=ORIENTED_EDGE('',*,*,#4556,.T.);
#6109=ORIENTED_EDGE('',*,*,#4557,.T.);
#6110=ORIENTED_EDGE('',*,*,#4556,.F.);
#6111=ORIENTED_EDGE('',*,*,#4557,.F.);
#6112=ORIENTED_EDGE('',*,*,#4558,.F.);
#6113=ORIENTED_EDGE('',*,*,#4559,.T.);
#6114=ORIENTED_EDGE('',*,*,#4560,.F.);
#6115=ORIENTED_EDGE('',*,*,#4561,.T.);
#6116=ORIENTED_EDGE('',*,*,#4558,.T.);
#6117=ORIENTED_EDGE('',*,*,#4561,.F.);
#6118=ORIENTED_EDGE('',*,*,#4560,.T.);
#6119=ORIENTED_EDGE('',*,*,#4554,.T.);
#6120=ORIENTED_EDGE('',*,*,#4559,.F.);
#6121=ORIENTED_EDGE('',*,*,#4562,.T.);
#6122=ORIENTED_EDGE('',*,*,#4563,.T.);
#6123=ORIENTED_EDGE('',*,*,#4562,.F.);
#6124=ORIENTED_EDGE('',*,*,#4563,.F.);
#6125=ORIENTED_EDGE('',*,*,#4555,.T.);
#6126=ORIENTED_EDGE('',*,*,#4564,.F.);
#6127=ORIENTED_EDGE('',*,*,#4565,.T.);
#6128=ORIENTED_EDGE('',*,*,#4566,.T.);
#6129=ORIENTED_EDGE('',*,*,#4565,.F.);
#6130=ORIENTED_EDGE('',*,*,#4567,.F.);
#6131=ORIENTED_EDGE('',*,*,#4568,.T.);
#6132=ORIENTED_EDGE('',*,*,#4569,.T.);
#6133=ORIENTED_EDGE('',*,*,#4568,.F.);
#6134=ORIENTED_EDGE('',*,*,#4567,.T.);
#6135=ORIENTED_EDGE('',*,*,#4564,.T.);
#6136=ORIENTED_EDGE('',*,*,#4569,.F.);
#6137=ORIENTED_EDGE('',*,*,#4566,.F.);
#6138=ORIENTED_EDGE('',*,*,#4570,.F.);
#6139=ORIENTED_EDGE('',*,*,#4571,.T.);
#6140=ORIENTED_EDGE('',*,*,#4572,.F.);
#6141=ORIENTED_EDGE('',*,*,#4571,.F.);
#6142=ORIENTED_EDGE('',*,*,#4573,.F.);
#6143=ORIENTED_EDGE('',*,*,#4574,.T.);
#6144=ORIENTED_EDGE('',*,*,#4575,.T.);
#6145=ORIENTED_EDGE('',*,*,#4574,.F.);
#6146=ORIENTED_EDGE('',*,*,#4575,.F.);
#6147=ORIENTED_EDGE('',*,*,#4576,.T.);
#6148=ORIENTED_EDGE('',*,*,#4577,.T.);
#6149=ORIENTED_EDGE('',*,*,#4578,.F.);
#6150=ORIENTED_EDGE('',*,*,#4579,.F.);
#6151=ORIENTED_EDGE('',*,*,#4572,.T.);
#6152=ORIENTED_EDGE('',*,*,#4580,.T.);
#6153=ORIENTED_EDGE('',*,*,#4579,.T.);
#6154=ORIENTED_EDGE('',*,*,#4581,.F.);
#6155=ORIENTED_EDGE('',*,*,#4582,.F.);
#6156=ORIENTED_EDGE('',*,*,#4583,.T.);
#6157=ORIENTED_EDGE('',*,*,#4582,.T.);
#6158=ORIENTED_EDGE('',*,*,#4584,.F.);
#6159=ORIENTED_EDGE('',*,*,#4585,.F.);
#6160=ORIENTED_EDGE('',*,*,#4570,.T.);
#6161=ORIENTED_EDGE('',*,*,#4586,.T.);
#6162=ORIENTED_EDGE('',*,*,#4585,.T.);
#6163=ORIENTED_EDGE('',*,*,#4587,.F.);
#6164=ORIENTED_EDGE('',*,*,#4577,.F.);
#6165=ORIENTED_EDGE('',*,*,#4573,.T.);
#6166=ORIENTED_EDGE('',*,*,#4587,.T.);
#6167=ORIENTED_EDGE('',*,*,#4584,.T.);
#6168=ORIENTED_EDGE('',*,*,#4581,.T.);
#6169=ORIENTED_EDGE('',*,*,#4578,.T.);
#6170=ORIENTED_EDGE('',*,*,#4586,.F.);
#6171=ORIENTED_EDGE('',*,*,#4576,.F.);
#6172=ORIENTED_EDGE('',*,*,#4580,.F.);
#6173=ORIENTED_EDGE('',*,*,#4583,.F.);
#6174=ORIENTED_EDGE('',*,*,#4588,.T.);
#6175=ORIENTED_EDGE('',*,*,#4589,.T.);
#6176=ORIENTED_EDGE('',*,*,#4590,.F.);
#6177=ORIENTED_EDGE('',*,*,#4591,.F.);
#6178=ORIENTED_EDGE('',*,*,#4592,.T.);
#6179=ORIENTED_EDGE('',*,*,#4591,.T.);
#6180=ORIENTED_EDGE('',*,*,#4593,.F.);
#6181=ORIENTED_EDGE('',*,*,#4594,.F.);
#6182=ORIENTED_EDGE('',*,*,#4595,.T.);
#6183=ORIENTED_EDGE('',*,*,#4594,.T.);
#6184=ORIENTED_EDGE('',*,*,#4596,.F.);
#6185=ORIENTED_EDGE('',*,*,#4597,.F.);
#6186=ORIENTED_EDGE('',*,*,#4598,.T.);
#6187=ORIENTED_EDGE('',*,*,#4597,.T.);
#6188=ORIENTED_EDGE('',*,*,#4599,.F.);
#6189=ORIENTED_EDGE('',*,*,#4589,.F.);
#6190=ORIENTED_EDGE('',*,*,#4599,.T.);
#6191=ORIENTED_EDGE('',*,*,#4596,.T.);
#6192=ORIENTED_EDGE('',*,*,#4593,.T.);
#6193=ORIENTED_EDGE('',*,*,#4590,.T.);
#6194=ORIENTED_EDGE('',*,*,#4598,.F.);
#6195=ORIENTED_EDGE('',*,*,#4588,.F.);
#6196=ORIENTED_EDGE('',*,*,#4592,.F.);
#6197=ORIENTED_EDGE('',*,*,#4595,.F.);
#6198=ORIENTED_EDGE('',*,*,#4600,.F.);
#6199=ORIENTED_EDGE('',*,*,#4601,.T.);
#6200=ORIENTED_EDGE('',*,*,#4602,.T.);
#6201=ORIENTED_EDGE('',*,*,#4601,.F.);
#6202=ORIENTED_EDGE('',*,*,#4600,.T.);
#6203=ORIENTED_EDGE('',*,*,#4602,.F.);
#6204=ORIENTED_EDGE('',*,*,#4603,.F.);
#6205=ORIENTED_EDGE('',*,*,#4603,.T.);
#6206=ORIENTED_EDGE('',*,*,#4604,.T.);
#6207=ORIENTED_EDGE('',*,*,#4605,.T.);
#6208=ORIENTED_EDGE('',*,*,#4604,.F.);
#6209=ORIENTED_EDGE('',*,*,#4605,.F.);
#6210=ORIENTED_EDGE('',*,*,#4606,.F.);
#6211=ORIENTED_EDGE('',*,*,#4607,.T.);
#6212=ORIENTED_EDGE('',*,*,#4608,.F.);
#6213=ORIENTED_EDGE('',*,*,#4609,.F.);
#6214=ORIENTED_EDGE('',*,*,#4610,.T.);
#6215=ORIENTED_EDGE('',*,*,#4611,.F.);
#6216=ORIENTED_EDGE('',*,*,#4610,.F.);
#6217=ORIENTED_EDGE('',*,*,#4612,.F.);
#6218=ORIENTED_EDGE('',*,*,#4613,.F.);
#6219=ORIENTED_EDGE('',*,*,#4607,.F.);
#6220=ORIENTED_EDGE('',*,*,#4614,.F.);
#6221=ORIENTED_EDGE('',*,*,#4615,.T.);
#6222=ORIENTED_EDGE('',*,*,#4616,.F.);
#6223=ORIENTED_EDGE('',*,*,#4617,.F.);
#6224=ORIENTED_EDGE('',*,*,#4618,.T.);
#6225=ORIENTED_EDGE('',*,*,#4619,.F.);
#6226=ORIENTED_EDGE('',*,*,#4618,.F.);
#6227=ORIENTED_EDGE('',*,*,#4620,.F.);
#6228=ORIENTED_EDGE('',*,*,#4621,.F.);
#6229=ORIENTED_EDGE('',*,*,#4615,.F.);
#6230=ORIENTED_EDGE('',*,*,#4622,.F.);
#6231=ORIENTED_EDGE('',*,*,#4623,.T.);
#6232=ORIENTED_EDGE('',*,*,#4624,.F.);
#6233=ORIENTED_EDGE('',*,*,#4625,.F.);
#6234=ORIENTED_EDGE('',*,*,#4626,.T.);
#6235=ORIENTED_EDGE('',*,*,#4627,.F.);
#6236=ORIENTED_EDGE('',*,*,#4626,.F.);
#6237=ORIENTED_EDGE('',*,*,#4628,.F.);
#6238=ORIENTED_EDGE('',*,*,#4629,.F.);
#6239=ORIENTED_EDGE('',*,*,#4623,.F.);
#6240=ORIENTED_EDGE('',*,*,#4630,.F.);
#6241=ORIENTED_EDGE('',*,*,#4631,.T.);
#6242=ORIENTED_EDGE('',*,*,#4632,.F.);
#6243=ORIENTED_EDGE('',*,*,#4633,.F.);
#6244=ORIENTED_EDGE('',*,*,#4634,.T.);
#6245=ORIENTED_EDGE('',*,*,#4635,.F.);
#6246=ORIENTED_EDGE('',*,*,#4634,.F.);
#6247=ORIENTED_EDGE('',*,*,#4636,.F.);
#6248=ORIENTED_EDGE('',*,*,#4637,.F.);
#6249=ORIENTED_EDGE('',*,*,#4631,.F.);
#6250=ORIENTED_EDGE('',*,*,#4608,.T.);
#6251=ORIENTED_EDGE('',*,*,#4606,.T.);
#6252=ORIENTED_EDGE('',*,*,#4613,.T.);
#6253=ORIENTED_EDGE('',*,*,#4638,.T.);
#6254=ORIENTED_EDGE('',*,*,#4624,.T.);
#6255=ORIENTED_EDGE('',*,*,#4622,.T.);
#6256=ORIENTED_EDGE('',*,*,#4629,.T.);
#6257=ORIENTED_EDGE('',*,*,#4639,.T.);
#6258=ORIENTED_EDGE('',*,*,#4640,.F.);
#6259=ORIENTED_EDGE('',*,*,#4641,.T.);
#6260=ORIENTED_EDGE('',*,*,#4642,.F.);
#6261=ORIENTED_EDGE('',*,*,#4643,.T.);
#6262=ORIENTED_EDGE('',*,*,#4616,.T.);
#6263=ORIENTED_EDGE('',*,*,#4614,.T.);
#6264=ORIENTED_EDGE('',*,*,#4621,.T.);
#6265=ORIENTED_EDGE('',*,*,#4644,.T.);
#6266=ORIENTED_EDGE('',*,*,#4632,.T.);
#6267=ORIENTED_EDGE('',*,*,#4630,.T.);
#6268=ORIENTED_EDGE('',*,*,#4637,.T.);
#6269=ORIENTED_EDGE('',*,*,#4645,.T.);
#6270=ORIENTED_EDGE('',*,*,#4646,.F.);
#6271=ORIENTED_EDGE('',*,*,#4647,.F.);
#6272=ORIENTED_EDGE('',*,*,#4648,.F.);
#6273=ORIENTED_EDGE('',*,*,#4649,.T.);
#6274=ORIENTED_EDGE('',*,*,#4640,.T.);
#6275=ORIENTED_EDGE('',*,*,#4650,.T.);
#6276=ORIENTED_EDGE('',*,*,#4651,.T.);
#6277=ORIENTED_EDGE('',*,*,#4652,.T.);
#6278=ORIENTED_EDGE('',*,*,#4653,.T.);
#6279=ORIENTED_EDGE('',*,*,#4654,.T.);
#6280=ORIENTED_EDGE('',*,*,#4648,.T.);
#6281=ORIENTED_EDGE('',*,*,#4655,.T.);
#6282=ORIENTED_EDGE('',*,*,#4656,.T.);
#6283=ORIENTED_EDGE('',*,*,#4657,.T.);
#6284=ORIENTED_EDGE('',*,*,#4658,.T.);
#6285=ORIENTED_EDGE('',*,*,#4659,.T.);
#6286=ORIENTED_EDGE('',*,*,#4612,.T.);
#6287=ORIENTED_EDGE('',*,*,#4609,.T.);
#6288=ORIENTED_EDGE('',*,*,#4643,.F.);
#6289=ORIENTED_EDGE('',*,*,#4660,.F.);
#6290=ORIENTED_EDGE('',*,*,#4661,.F.);
#6291=ORIENTED_EDGE('',*,*,#4650,.F.);
#6292=ORIENTED_EDGE('',*,*,#4639,.F.);
#6293=ORIENTED_EDGE('',*,*,#4628,.T.);
#6294=ORIENTED_EDGE('',*,*,#4625,.T.);
#6295=ORIENTED_EDGE('',*,*,#4638,.F.);
#6296=ORIENTED_EDGE('',*,*,#4661,.T.);
#6297=ORIENTED_EDGE('',*,*,#4662,.F.);
#6298=ORIENTED_EDGE('',*,*,#4663,.F.);
#6299=ORIENTED_EDGE('',*,*,#4651,.F.);
#6300=ORIENTED_EDGE('',*,*,#4663,.T.);
#6301=ORIENTED_EDGE('',*,*,#4664,.F.);
#6302=ORIENTED_EDGE('',*,*,#4665,.F.);
#6303=ORIENTED_EDGE('',*,*,#4652,.F.);
#6304=ORIENTED_EDGE('',*,*,#4611,.T.);
#6305=ORIENTED_EDGE('',*,*,#4619,.T.);
#6306=ORIENTED_EDGE('',*,*,#4627,.T.);
#6307=ORIENTED_EDGE('',*,*,#4635,.T.);
#6308=ORIENTED_EDGE('',*,*,#4665,.T.);
#6309=ORIENTED_EDGE('',*,*,#4666,.F.);
#6310=ORIENTED_EDGE('',*,*,#4667,.F.);
#6311=ORIENTED_EDGE('',*,*,#4653,.F.);
#6312=ORIENTED_EDGE('',*,*,#4620,.T.);
#6313=ORIENTED_EDGE('',*,*,#4617,.T.);
#6314=ORIENTED_EDGE('',*,*,#4649,.F.);
#6315=ORIENTED_EDGE('',*,*,#4654,.F.);
#6316=ORIENTED_EDGE('',*,*,#4667,.T.);
#6317=ORIENTED_EDGE('',*,*,#4668,.F.);
#6318=ORIENTED_EDGE('',*,*,#4645,.F.);
#6319=ORIENTED_EDGE('',*,*,#4636,.T.);
#6320=ORIENTED_EDGE('',*,*,#4633,.T.);
#6321=ORIENTED_EDGE('',*,*,#4644,.F.);
#6322=ORIENTED_EDGE('',*,*,#4647,.T.);
#6323=ORIENTED_EDGE('',*,*,#4669,.F.);
#6324=ORIENTED_EDGE('',*,*,#4670,.F.);
#6325=ORIENTED_EDGE('',*,*,#4655,.F.);
#6326=ORIENTED_EDGE('',*,*,#4670,.T.);
#6327=ORIENTED_EDGE('',*,*,#4671,.F.);
#6328=ORIENTED_EDGE('',*,*,#4672,.F.);
#6329=ORIENTED_EDGE('',*,*,#4656,.F.);
#6330=ORIENTED_EDGE('',*,*,#4672,.T.);
#6331=ORIENTED_EDGE('',*,*,#4673,.F.);
#6332=ORIENTED_EDGE('',*,*,#4674,.F.);
#6333=ORIENTED_EDGE('',*,*,#4657,.F.);
#6334=ORIENTED_EDGE('',*,*,#4674,.T.);
#6335=ORIENTED_EDGE('',*,*,#4675,.F.);
#6336=ORIENTED_EDGE('',*,*,#4676,.F.);
#6337=ORIENTED_EDGE('',*,*,#4658,.F.);
#6338=ORIENTED_EDGE('',*,*,#4676,.T.);
#6339=ORIENTED_EDGE('',*,*,#4677,.F.);
#6340=ORIENTED_EDGE('',*,*,#4641,.F.);
#6341=ORIENTED_EDGE('',*,*,#4659,.F.);
#6342=ORIENTED_EDGE('',*,*,#4642,.T.);
#6343=ORIENTED_EDGE('',*,*,#4677,.T.);
#6344=ORIENTED_EDGE('',*,*,#4675,.T.);
#6345=ORIENTED_EDGE('',*,*,#4673,.T.);
#6346=ORIENTED_EDGE('',*,*,#4671,.T.);
#6347=ORIENTED_EDGE('',*,*,#4669,.T.);
#6348=ORIENTED_EDGE('',*,*,#4646,.T.);
#6349=ORIENTED_EDGE('',*,*,#4668,.T.);
#6350=ORIENTED_EDGE('',*,*,#4666,.T.);
#6351=ORIENTED_EDGE('',*,*,#4664,.T.);
#6352=ORIENTED_EDGE('',*,*,#4662,.T.);
#6353=ORIENTED_EDGE('',*,*,#4660,.T.);
#6354=ORIENTED_EDGE('',*,*,#4678,.T.);
#6355=ORIENTED_EDGE('',*,*,#4679,.T.);
#6356=ORIENTED_EDGE('',*,*,#4680,.F.);
#6357=ORIENTED_EDGE('',*,*,#4681,.F.);
#6358=ORIENTED_EDGE('',*,*,#4682,.T.);
#6359=ORIENTED_EDGE('',*,*,#4681,.T.);
#6360=ORIENTED_EDGE('',*,*,#4683,.F.);
#6361=ORIENTED_EDGE('',*,*,#4684,.F.);
#6362=ORIENTED_EDGE('',*,*,#4685,.T.);
#6363=ORIENTED_EDGE('',*,*,#4684,.T.);
#6364=ORIENTED_EDGE('',*,*,#4686,.F.);
#6365=ORIENTED_EDGE('',*,*,#4687,.F.);
#6366=ORIENTED_EDGE('',*,*,#4688,.T.);
#6367=ORIENTED_EDGE('',*,*,#4687,.T.);
#6368=ORIENTED_EDGE('',*,*,#4689,.F.);
#6369=ORIENTED_EDGE('',*,*,#4690,.F.);
#6370=ORIENTED_EDGE('',*,*,#4691,.T.);
#6371=ORIENTED_EDGE('',*,*,#4690,.T.);
#6372=ORIENTED_EDGE('',*,*,#4692,.F.);
#6373=ORIENTED_EDGE('',*,*,#4693,.F.);
#6374=ORIENTED_EDGE('',*,*,#4694,.T.);
#6375=ORIENTED_EDGE('',*,*,#4693,.T.);
#6376=ORIENTED_EDGE('',*,*,#4695,.F.);
#6377=ORIENTED_EDGE('',*,*,#4696,.F.);
#6378=ORIENTED_EDGE('',*,*,#4697,.T.);
#6379=ORIENTED_EDGE('',*,*,#4696,.T.);
#6380=ORIENTED_EDGE('',*,*,#4698,.F.);
#6381=ORIENTED_EDGE('',*,*,#4699,.F.);
#6382=ORIENTED_EDGE('',*,*,#4700,.T.);
#6383=ORIENTED_EDGE('',*,*,#4699,.T.);
#6384=ORIENTED_EDGE('',*,*,#4701,.F.);
#6385=ORIENTED_EDGE('',*,*,#4679,.F.);
#6386=ORIENTED_EDGE('',*,*,#4701,.T.);
#6387=ORIENTED_EDGE('',*,*,#4698,.T.);
#6388=ORIENTED_EDGE('',*,*,#4695,.T.);
#6389=ORIENTED_EDGE('',*,*,#4692,.T.);
#6390=ORIENTED_EDGE('',*,*,#4689,.T.);
#6391=ORIENTED_EDGE('',*,*,#4686,.T.);
#6392=ORIENTED_EDGE('',*,*,#4683,.T.);
#6393=ORIENTED_EDGE('',*,*,#4680,.T.);
#6394=ORIENTED_EDGE('',*,*,#4700,.F.);
#6395=ORIENTED_EDGE('',*,*,#4678,.F.);
#6396=ORIENTED_EDGE('',*,*,#4682,.F.);
#6397=ORIENTED_EDGE('',*,*,#4685,.F.);
#6398=ORIENTED_EDGE('',*,*,#4688,.F.);
#6399=ORIENTED_EDGE('',*,*,#4691,.F.);
#6400=ORIENTED_EDGE('',*,*,#4694,.F.);
#6401=ORIENTED_EDGE('',*,*,#4697,.F.);
#6402=ORIENTED_EDGE('',*,*,#4702,.F.);
#6403=ORIENTED_EDGE('',*,*,#4703,.T.);
#6404=ORIENTED_EDGE('',*,*,#4704,.F.);
#6405=ORIENTED_EDGE('',*,*,#4705,.F.);
#6406=ORIENTED_EDGE('',*,*,#4706,.F.);
#6407=ORIENTED_EDGE('',*,*,#4705,.T.);
#6408=ORIENTED_EDGE('',*,*,#4707,.F.);
#6409=ORIENTED_EDGE('',*,*,#4708,.F.);
#6410=ORIENTED_EDGE('',*,*,#4709,.F.);
#6411=ORIENTED_EDGE('',*,*,#4708,.T.);
#6412=ORIENTED_EDGE('',*,*,#4710,.F.);
#6413=ORIENTED_EDGE('',*,*,#4711,.F.);
#6414=ORIENTED_EDGE('',*,*,#4712,.F.);
#6415=ORIENTED_EDGE('',*,*,#4711,.T.);
#6416=ORIENTED_EDGE('',*,*,#4713,.F.);
#6417=ORIENTED_EDGE('',*,*,#4714,.F.);
#6418=ORIENTED_EDGE('',*,*,#4715,.F.);
#6419=ORIENTED_EDGE('',*,*,#4714,.T.);
#6420=ORIENTED_EDGE('',*,*,#4716,.F.);
#6421=ORIENTED_EDGE('',*,*,#4717,.F.);
#6422=ORIENTED_EDGE('',*,*,#4718,.F.);
#6423=ORIENTED_EDGE('',*,*,#4717,.T.);
#6424=ORIENTED_EDGE('',*,*,#4719,.F.);
#6425=ORIENTED_EDGE('',*,*,#4720,.F.);
#6426=ORIENTED_EDGE('',*,*,#4721,.F.);
#6427=ORIENTED_EDGE('',*,*,#4720,.T.);
#6428=ORIENTED_EDGE('',*,*,#4722,.F.);
#6429=ORIENTED_EDGE('',*,*,#4723,.F.);
#6430=ORIENTED_EDGE('',*,*,#4724,.F.);
#6431=ORIENTED_EDGE('',*,*,#4723,.T.);
#6432=ORIENTED_EDGE('',*,*,#4725,.F.);
#6433=ORIENTED_EDGE('',*,*,#4703,.F.);
#6434=ORIENTED_EDGE('',*,*,#4724,.T.);
#6435=ORIENTED_EDGE('',*,*,#4702,.T.);
#6436=ORIENTED_EDGE('',*,*,#4706,.T.);
#6437=ORIENTED_EDGE('',*,*,#4709,.T.);
#6438=ORIENTED_EDGE('',*,*,#4712,.T.);
#6439=ORIENTED_EDGE('',*,*,#4715,.T.);
#6440=ORIENTED_EDGE('',*,*,#4718,.T.);
#6441=ORIENTED_EDGE('',*,*,#4721,.T.);
#6442=ORIENTED_EDGE('',*,*,#4725,.T.);
#6443=ORIENTED_EDGE('',*,*,#4722,.T.);
#6444=ORIENTED_EDGE('',*,*,#4719,.T.);
#6445=ORIENTED_EDGE('',*,*,#4716,.T.);
#6446=ORIENTED_EDGE('',*,*,#4713,.T.);
#6447=ORIENTED_EDGE('',*,*,#4710,.T.);
#6448=ORIENTED_EDGE('',*,*,#4707,.T.);
#6449=ORIENTED_EDGE('',*,*,#4704,.T.);
#6450=ORIENTED_EDGE('',*,*,#4726,.T.);
#6451=ORIENTED_EDGE('',*,*,#4727,.T.);
#6452=ORIENTED_EDGE('',*,*,#4728,.T.);
#6453=ORIENTED_EDGE('',*,*,#4729,.F.);
#6454=ORIENTED_EDGE('',*,*,#4730,.T.);
#6455=ORIENTED_EDGE('',*,*,#4731,.T.);
#6456=ORIENTED_EDGE('',*,*,#4732,.T.);
#6457=ORIENTED_EDGE('',*,*,#4727,.F.);
#6458=ORIENTED_EDGE('',*,*,#4733,.T.);
#6459=ORIENTED_EDGE('',*,*,#4734,.T.);
#6460=ORIENTED_EDGE('',*,*,#4735,.T.);
#6461=ORIENTED_EDGE('',*,*,#4731,.F.);
#6462=ORIENTED_EDGE('',*,*,#4736,.T.);
#6463=ORIENTED_EDGE('',*,*,#4737,.T.);
#6464=ORIENTED_EDGE('',*,*,#4738,.T.);
#6465=ORIENTED_EDGE('',*,*,#4734,.F.);
#6466=ORIENTED_EDGE('',*,*,#4739,.T.);
#6467=ORIENTED_EDGE('',*,*,#4740,.T.);
#6468=ORIENTED_EDGE('',*,*,#4741,.T.);
#6469=ORIENTED_EDGE('',*,*,#4737,.F.);
#6470=ORIENTED_EDGE('',*,*,#4742,.T.);
#6471=ORIENTED_EDGE('',*,*,#4729,.T.);
#6472=ORIENTED_EDGE('',*,*,#4743,.T.);
#6473=ORIENTED_EDGE('',*,*,#4740,.F.);
#6474=ORIENTED_EDGE('',*,*,#4742,.F.);
#6475=ORIENTED_EDGE('',*,*,#4739,.F.);
#6476=ORIENTED_EDGE('',*,*,#4736,.F.);
#6477=ORIENTED_EDGE('',*,*,#4733,.F.);
#6478=ORIENTED_EDGE('',*,*,#4730,.F.);
#6479=ORIENTED_EDGE('',*,*,#4726,.F.);
#6480=ORIENTED_EDGE('',*,*,#4743,.F.);
#6481=ORIENTED_EDGE('',*,*,#4728,.F.);
#6482=ORIENTED_EDGE('',*,*,#4732,.F.);
#6483=ORIENTED_EDGE('',*,*,#4735,.F.);
#6484=ORIENTED_EDGE('',*,*,#4738,.F.);
#6485=ORIENTED_EDGE('',*,*,#4741,.F.);
#6486=ORIENTED_EDGE('',*,*,#4744,.F.);
#6487=ORIENTED_EDGE('',*,*,#4745,.F.);
#6488=ORIENTED_EDGE('',*,*,#4746,.F.);
#6489=ORIENTED_EDGE('',*,*,#4747,.T.);
#6490=ORIENTED_EDGE('',*,*,#4745,.T.);
#6491=ORIENTED_EDGE('',*,*,#4747,.F.);
#6492=ORIENTED_EDGE('',*,*,#4748,.F.);
#6493=ORIENTED_EDGE('',*,*,#4749,.T.);
#6494=ORIENTED_EDGE('',*,*,#4746,.T.);
#6495=ORIENTED_EDGE('',*,*,#4749,.F.);
#6496=ORIENTED_EDGE('',*,*,#4750,.F.);
#6497=ORIENTED_EDGE('',*,*,#4751,.T.);
#6498=ORIENTED_EDGE('',*,*,#4748,.T.);
#6499=ORIENTED_EDGE('',*,*,#4751,.F.);
#6500=ORIENTED_EDGE('',*,*,#4750,.T.);
#6501=ORIENTED_EDGE('',*,*,#4752,.F.);
#6502=ORIENTED_EDGE('',*,*,#4753,.F.);
#6503=ORIENTED_EDGE('',*,*,#4754,.T.);
#6504=ORIENTED_EDGE('',*,*,#4752,.T.);
#6505=ORIENTED_EDGE('',*,*,#4754,.F.);
#6506=ORIENTED_EDGE('',*,*,#4744,.T.);
#6507=ORIENTED_EDGE('',*,*,#4755,.T.);
#6508=ORIENTED_EDGE('',*,*,#4753,.T.);
#6509=ORIENTED_EDGE('',*,*,#4755,.F.);
#6510=ORIENTED_EDGE('',*,*,#4756,.F.);
#6511=ORIENTED_EDGE('',*,*,#4757,.F.);
#6512=ORIENTED_EDGE('',*,*,#4758,.T.);
#6513=ORIENTED_EDGE('',*,*,#4756,.T.);
#6514=ORIENTED_EDGE('',*,*,#4758,.F.);
#6515=ORIENTED_EDGE('',*,*,#4759,.F.);
#6516=ORIENTED_EDGE('',*,*,#4760,.T.);
#6517=ORIENTED_EDGE('',*,*,#4757,.T.);
#6518=ORIENTED_EDGE('',*,*,#4760,.F.);
#6519=ORIENTED_EDGE('',*,*,#4761,.F.);
#6520=ORIENTED_EDGE('',*,*,#4762,.T.);
#6521=ORIENTED_EDGE('',*,*,#4759,.T.);
#6522=ORIENTED_EDGE('',*,*,#4762,.F.);
#6523=ORIENTED_EDGE('',*,*,#4761,.T.);
#6524=ORIENTED_EDGE('',*,*,#4763,.F.);
#6525=ORIENTED_EDGE('',*,*,#4764,.F.);
#6526=ORIENTED_EDGE('',*,*,#4765,.T.);
#6527=ORIENTED_EDGE('',*,*,#4763,.T.);
#6528=ORIENTED_EDGE('',*,*,#4765,.F.);
#6529=ORIENTED_EDGE('',*,*,#4766,.F.);
#6530=ORIENTED_EDGE('',*,*,#4767,.T.);
#6531=ORIENTED_EDGE('',*,*,#4764,.T.);
#6532=ORIENTED_EDGE('',*,*,#4767,.F.);
#6533=ORIENTED_EDGE('',*,*,#4768,.F.);
#6534=ORIENTED_EDGE('',*,*,#4769,.T.);
#6535=ORIENTED_EDGE('',*,*,#4766,.T.);
#6536=ORIENTED_EDGE('',*,*,#4769,.F.);
#6537=ORIENTED_EDGE('',*,*,#4768,.T.);
#6538=ORIENTED_EDGE('',*,*,#4770,.T.);
#6539=ORIENTED_EDGE('',*,*,#4771,.T.);
#6540=ORIENTED_EDGE('',*,*,#4772,.T.);
#6541=ORIENTED_EDGE('',*,*,#4773,.F.);
#6542=ORIENTED_EDGE('',*,*,#4774,.T.);
#6543=ORIENTED_EDGE('',*,*,#4775,.T.);
#6544=ORIENTED_EDGE('',*,*,#4776,.T.);
#6545=ORIENTED_EDGE('',*,*,#4771,.F.);
#6546=ORIENTED_EDGE('',*,*,#4777,.T.);
#6547=ORIENTED_EDGE('',*,*,#4778,.T.);
#6548=ORIENTED_EDGE('',*,*,#4779,.T.);
#6549=ORIENTED_EDGE('',*,*,#4775,.F.);
#6550=ORIENTED_EDGE('',*,*,#4780,.T.);
#6551=ORIENTED_EDGE('',*,*,#4781,.T.);
#6552=ORIENTED_EDGE('',*,*,#4782,.T.);
#6553=ORIENTED_EDGE('',*,*,#4778,.F.);
#6554=ORIENTED_EDGE('',*,*,#4783,.T.);
#6555=ORIENTED_EDGE('',*,*,#4784,.T.);
#6556=ORIENTED_EDGE('',*,*,#4785,.T.);
#6557=ORIENTED_EDGE('',*,*,#4781,.F.);
#6558=ORIENTED_EDGE('',*,*,#4786,.T.);
#6559=ORIENTED_EDGE('',*,*,#4773,.T.);
#6560=ORIENTED_EDGE('',*,*,#4787,.T.);
#6561=ORIENTED_EDGE('',*,*,#4784,.F.);
#6562=ORIENTED_EDGE('',*,*,#4786,.F.);
#6563=ORIENTED_EDGE('',*,*,#4783,.F.);
#6564=ORIENTED_EDGE('',*,*,#4780,.F.);
#6565=ORIENTED_EDGE('',*,*,#4777,.F.);
#6566=ORIENTED_EDGE('',*,*,#4774,.F.);
#6567=ORIENTED_EDGE('',*,*,#4770,.F.);
#6568=ORIENTED_EDGE('',*,*,#4787,.F.);
#6569=ORIENTED_EDGE('',*,*,#4772,.F.);
#6570=ORIENTED_EDGE('',*,*,#4776,.F.);
#6571=ORIENTED_EDGE('',*,*,#4779,.F.);
#6572=ORIENTED_EDGE('',*,*,#4782,.F.);
#6573=ORIENTED_EDGE('',*,*,#4785,.F.);
#6574=CYLINDRICAL_SURFACE('',#7501,0.21);
#6575=CYLINDRICAL_SURFACE('',#7505,0.21);
#6576=CYLINDRICAL_SURFACE('',#7509,0.165);
#6577=CYLINDRICAL_SURFACE('',#7513,0.164999999999999);
#6578=CYLINDRICAL_SURFACE('',#7517,0.275);
#6579=CYLINDRICAL_SURFACE('',#7541,0.275);
#6580=CYLINDRICAL_SURFACE('',#7551,0.210000000000001);
#6581=CYLINDRICAL_SURFACE('',#7554,0.210000000000001);
#6582=CYLINDRICAL_SURFACE('',#7557,0.164999999999999);
#6583=CYLINDRICAL_SURFACE('',#7560,0.164999999999999);
#6584=CYLINDRICAL_SURFACE('',#7563,0.164999999999999);
#6585=CYLINDRICAL_SURFACE('',#7566,0.164999999999999);
#6586=CYLINDRICAL_SURFACE('',#7569,0.274999999999999);
#6587=CYLINDRICAL_SURFACE('',#7572,0.275);
#6588=CYLINDRICAL_SURFACE('',#7586,0.275);
#6589=CYLINDRICAL_SURFACE('',#7596,0.274999999999999);
#6590=CYLINDRICAL_SURFACE('',#7606,0.225);
#6591=CYLINDRICAL_SURFACE('',#7609,0.225);
#6592=CYLINDRICAL_SURFACE('',#7612,1.1);
#6593=CYLINDRICAL_SURFACE('',#7615,1.5);
#6594=CYLINDRICAL_SURFACE('',#7621,2.2);
#6595=CYLINDRICAL_SURFACE('',#7626,1.1);
#6596=CYLINDRICAL_SURFACE('',#7629,1.3);
#6597=CYLINDRICAL_SURFACE('',#7635,0.225);
#6598=CYLINDRICAL_SURFACE('',#7638,0.225);
#6599=CYLINDRICAL_SURFACE('',#7641,1.01);
#6600=CYLINDRICAL_SURFACE('',#7646,1.09);
#6601=CYLINDRICAL_SURFACE('',#7651,0.605);
#6602=CYLINDRICAL_SURFACE('',#7652,2.2);
#6603=CYLINDRICAL_SURFACE('',#7664,0.300000000000001);
#6604=CYLINDRICAL_SURFACE('',#7665,0.199999999999999);
#6605=CYLINDRICAL_SURFACE('',#7667,0.199999999999999);
#6606=CYLINDRICAL_SURFACE('',#7672,0.164999999999999);
#6607=CYLINDRICAL_SURFACE('',#7675,0.4);
#6608=CYLINDRICAL_SURFACE('',#7687,0.3);
#6609=CYLINDRICAL_SURFACE('',#7688,0.2);
#6610=CYLINDRICAL_SURFACE('',#7690,0.2);
#6611=CYLINDRICAL_SURFACE('',#7695,0.165);
#6612=CYLINDRICAL_SURFACE('',#7698,0.4);
#6613=CYLINDRICAL_SURFACE('',#7709,0.5);
#6614=CYLINDRICAL_SURFACE('',#7718,0.275);
#6615=CYLINDRICAL_SURFACE('',#7723,0.5);
#6616=CYLINDRICAL_SURFACE('',#7724,0.275);
#6617=CYLINDRICAL_SURFACE('',#7731,0.5);
#6618=CYLINDRICAL_SURFACE('',#7740,0.275);
#6619=CYLINDRICAL_SURFACE('',#7745,0.5);
#6620=CYLINDRICAL_SURFACE('',#7746,0.275);
#6621=CYLINDRICAL_SURFACE('',#7789,0.21);
#6622=CYLINDRICAL_SURFACE('',#7803,0.375);
#6623=CYLINDRICAL_SURFACE('',#7808,0.375);
#6624=CYLINDRICAL_SURFACE('',#7813,0.375);
#6625=CYLINDRICAL_SURFACE('',#7818,0.375);
#6626=CYLINDRICAL_SURFACE('',#7823,0.225);
#6627=CYLINDRICAL_SURFACE('',#7825,0.225);
#6628=CYLINDRICAL_SURFACE('',#7827,0.225);
#6629=CYLINDRICAL_SURFACE('',#7829,0.225000000000001);
#6630=CYLINDRICAL_SURFACE('',#7857,0.25);
#6631=CYLINDRICAL_SURFACE('',#7864,0.425);
#6632=CYLINDRICAL_SURFACE('',#7872,0.24505);
#6633=CYLINDRICAL_SURFACE('',#7878,0.425);
#6634=CYLINDRICAL_SURFACE('',#7886,0.24505);
#6635=CYLINDRICAL_SURFACE('',#7911,0.2117);
#6636=CYLINDRICAL_SURFACE('',#7924,0.265);
#6637=CYLINDRICAL_SURFACE('',#7928,0.5);
#6638=CYLINDRICAL_SURFACE('',#7933,0.225000000000001);
#6639=CYLINDRICAL_SURFACE('',#7941,0.525);
#6640=CYLINDRICAL_SURFACE('',#7944,0.45);
#6641=CYLINDRICAL_SURFACE('',#7947,0.449999999999999);
#6642=CYLINDRICAL_SURFACE('',#7950,0.5);
#6643=CYLINDRICAL_SURFACE('',#7960,0.274999999999999);
#6644=CYLINDRICAL_SURFACE('',#7963,0.274999999999999);
#6645=CYLINDRICAL_SURFACE('',#7965,0.5);
#6646=CYLINDRICAL_SURFACE('',#7968,0.274999999999999);
#6647=CYLINDRICAL_SURFACE('',#7970,0.274999999999999);
#6648=CYLINDRICAL_SURFACE('',#7984,0.425);
#6649=CYLINDRICAL_SURFACE('',#7987,1.09);
#6650=CYLINDRICAL_SURFACE('',#7993,0.5);
#6651=CYLINDRICAL_SURFACE('',#7997,0.5);
#6652=CYLINDRICAL_SURFACE('',#8004,1.);
#6653=CYLINDRICAL_SURFACE('',#8007,0.6);
#6654=CYLINDRICAL_SURFACE('',#8011,0.425);
#6655=CYLINDRICAL_SURFACE('',#8014,0.9);
#6656=CYLINDRICAL_SURFACE('',#8020,0.25);
#6657=CYLINDRICAL_SURFACE('',#8023,0.164999999999999);
#6658=CYLINDRICAL_SURFACE('',#8041,1.2);
#6659=CYLINDRICAL_SURFACE('',#8047,0.3);
#6660=CYLINDRICAL_SURFACE('',#8054,0.21);
#6661=CYLINDRICAL_SURFACE('',#8060,0.21);
#6662=CYLINDRICAL_SURFACE('',#8066,0.21);
#6663=CYLINDRICAL_SURFACE('',#8072,0.21);
#6664=CYLINDRICAL_SURFACE('',#8130,0.425);
#6665=CYLINDRICAL_SURFACE('',#8138,0.24505);
#6666=CYLINDRICAL_SURFACE('',#8144,0.35);
#6667=CYLINDRICAL_SURFACE('',#8152,0.1954);
#6668=ADVANCED_FACE('',(#826),#6574,.F.);
#6669=ADVANCED_FACE('',(#827),#531,.T.);
#6670=ADVANCED_FACE('',(#828),#6575,.F.);
#6671=ADVANCED_FACE('',(#829),#532,.T.);
#6672=ADVANCED_FACE('',(#830),#6576,.F.);
#6673=ADVANCED_FACE('',(#831),#533,.T.);
#6674=ADVANCED_FACE('',(#832),#6577,.F.);
#6675=ADVANCED_FACE('',(#833),#534,.T.);
#6676=ADVANCED_FACE('',(#834),#6578,.F.);
#6677=ADVANCED_FACE('',(#835),#535,.T.);
#6678=ADVANCED_FACE('',(#836),#536,.T.);
#6679=ADVANCED_FACE('',(#837),#537,.T.);
#6680=ADVANCED_FACE('',(#838),#538,.T.);
#6681=ADVANCED_FACE('',(#839,#416,#417,#418,#419,#420),#539,.T.);
#6682=ADVANCED_FACE('',(#840,#421),#540,.F.);
#6683=ADVANCED_FACE('',(#841),#541,.T.);
#6684=ADVANCED_FACE('',(#842),#542,.T.);
#6685=ADVANCED_FACE('',(#843),#543,.T.);
#6686=ADVANCED_FACE('',(#844),#544,.T.);
#6687=ADVANCED_FACE('',(#845),#545,.T.);
#6688=ADVANCED_FACE('',(#846),#546,.F.);
#6689=ADVANCED_FACE('',(#847),#547,.T.);
#6690=ADVANCED_FACE('',(#848),#548,.T.);
#6691=ADVANCED_FACE('',(#849),#549,.T.);
#6692=ADVANCED_FACE('',(#850),#550,.T.);
#6693=ADVANCED_FACE('',(#851),#551,.T.);
#6694=ADVANCED_FACE('',(#852),#552,.F.);
#6695=ADVANCED_FACE('',(#853),#6579,.F.);
#6696=ADVANCED_FACE('',(#854),#553,.T.);
#6697=ADVANCED_FACE('',(#855),#554,.T.);
#6698=ADVANCED_FACE('',(#856),#555,.T.);
#6699=ADVANCED_FACE('',(#857),#556,.T.);
#6700=ADVANCED_FACE('',(#858,#422),#557,.T.);
#6701=ADVANCED_FACE('',(#859,#423),#558,.F.);
#6702=ADVANCED_FACE('',(#860),#6580,.F.);
#6703=ADVANCED_FACE('',(#861),#6581,.F.);
#6704=ADVANCED_FACE('',(#862),#6582,.F.);
#6705=ADVANCED_FACE('',(#863),#6583,.F.);
#6706=ADVANCED_FACE('',(#864),#6584,.F.);
#6707=ADVANCED_FACE('',(#865),#6585,.F.);
#6708=ADVANCED_FACE('',(#866),#6586,.F.);
#6709=ADVANCED_FACE('',(#867),#6587,.F.);
#6710=ADVANCED_FACE('',(#868),#559,.F.);
#6711=ADVANCED_FACE('',(#869),#560,.F.);
#6712=ADVANCED_FACE('',(#870),#561,.F.);
#6713=ADVANCED_FACE('',(#871,#424,#425,#426,#427,#428,#429,#430,#431),#562,
 .T.);
#6714=ADVANCED_FACE('',(#872),#563,.T.);
#6715=ADVANCED_FACE('',(#873),#564,.T.);
#6716=ADVANCED_FACE('',(#874,#432,#433,#434,#435,#436,#437,#438,#439),#565,
 .T.);
#6717=ADVANCED_FACE('',(#875),#566,.T.);
#6718=ADVANCED_FACE('',(#876),#567,.T.);
#6719=ADVANCED_FACE('',(#877),#568,.F.);
#6720=ADVANCED_FACE('',(#878),#6588,.F.);
#6721=ADVANCED_FACE('',(#879),#569,.T.);
#6722=ADVANCED_FACE('',(#880,#440),#570,.T.);
#6723=ADVANCED_FACE('',(#881),#571,.T.);
#6724=ADVANCED_FACE('',(#882,#441),#572,.T.);
#6725=ADVANCED_FACE('',(#883),#573,.T.);
#6726=ADVANCED_FACE('',(#884),#574,.F.);
#6727=ADVANCED_FACE('',(#885),#6589,.F.);
#6728=ADVANCED_FACE('',(#886),#575,.T.);
#6729=ADVANCED_FACE('',(#887,#442),#576,.T.);
#6730=ADVANCED_FACE('',(#888),#577,.T.);
#6731=ADVANCED_FACE('',(#889,#443),#578,.T.);
#6732=ADVANCED_FACE('',(#890),#579,.T.);
#6733=ADVANCED_FACE('',(#891),#580,.F.);
#6734=ADVANCED_FACE('',(#892),#6590,.F.);
#6735=ADVANCED_FACE('',(#893),#6591,.F.);
#6736=ADVANCED_FACE('',(#894),#6592,.F.);
#6737=ADVANCED_FACE('',(#895),#6593,.T.);
#6738=ADVANCED_FACE('',(#896,#444),#581,.T.);
#6739=ADVANCED_FACE('',(#897,#445,#446,#447),#582,.T.);
#6740=ADVANCED_FACE('',(#898),#6594,.T.);
#6741=ADVANCED_FACE('',(#899),#583,.T.);
#6742=ADVANCED_FACE('',(#900,#448,#449),#584,.F.);
#6743=ADVANCED_FACE('',(#901),#6595,.F.);
#6744=ADVANCED_FACE('',(#902),#6596,.T.);
#6745=ADVANCED_FACE('',(#903,#450),#585,.T.);
#6746=ADVANCED_FACE('',(#904,#451),#586,.F.);
#6747=ADVANCED_FACE('',(#905),#6597,.F.);
#6748=ADVANCED_FACE('',(#906),#6598,.F.);
#6749=ADVANCED_FACE('',(#907),#6599,.F.);
#6750=ADVANCED_FACE('',(#908,#452),#587,.T.);
#6751=ADVANCED_FACE('',(#909),#6600,.T.);
#6752=ADVANCED_FACE('',(#910,#453),#588,.F.);
#6753=ADVANCED_FACE('',(#911),#6601,.F.);
#6754=ADVANCED_FACE('',(#912),#6602,.T.);
#6755=ADVANCED_FACE('',(#913,#454,#455,#456),#589,.T.);
#6756=ADVANCED_FACE('',(#914,#457,#458,#459),#590,.F.);
#6757=ADVANCED_FACE('',(#915,#460),#591,.T.);
#6758=ADVANCED_FACE('',(#916,#461),#592,.F.);
#6759=ADVANCED_FACE('',(#917),#6603,.T.);
#6760=ADVANCED_FACE('',(#918),#6604,.T.);
#6761=ADVANCED_FACE('',(#919),#6605,.T.);
#6762=ADVANCED_FACE('',(#920),#593,.T.);
#6763=ADVANCED_FACE('',(#921),#594,.F.);
#6764=ADVANCED_FACE('',(#922),#6606,.F.);
#6765=ADVANCED_FACE('',(#923),#6607,.T.);
#6766=ADVANCED_FACE('',(#924,#462),#595,.T.);
#6767=ADVANCED_FACE('',(#925,#463),#596,.F.);
#6768=ADVANCED_FACE('',(#926,#464),#597,.T.);
#6769=ADVANCED_FACE('',(#927,#465),#598,.F.);
#6770=ADVANCED_FACE('',(#928),#6608,.T.);
#6771=ADVANCED_FACE('',(#929),#6609,.T.);
#6772=ADVANCED_FACE('',(#930),#6610,.T.);
#6773=ADVANCED_FACE('',(#931),#599,.T.);
#6774=ADVANCED_FACE('',(#932),#600,.F.);
#6775=ADVANCED_FACE('',(#933),#6611,.F.);
#6776=ADVANCED_FACE('',(#934),#6612,.T.);
#6777=ADVANCED_FACE('',(#935,#466),#601,.T.);
#6778=ADVANCED_FACE('',(#936,#467),#602,.F.);
#6779=ADVANCED_FACE('',(#937),#279,.T.);
#6780=ADVANCED_FACE('',(#938),#603,.T.);
#6781=ADVANCED_FACE('',(#939),#604,.F.);
#6782=ADVANCED_FACE('',(#940),#6613,.F.);
#6783=ADVANCED_FACE('',(#941),#605,.F.);
#6784=ADVANCED_FACE('',(#942,#468,#469),#606,.T.);
#6785=ADVANCED_FACE('',(#943),#6614,.F.);
#6786=ADVANCED_FACE('',(#944,#470),#607,.T.);
#6787=ADVANCED_FACE('',(#945),#6615,.F.);
#6788=ADVANCED_FACE('',(#946),#6616,.F.);
#6789=ADVANCED_FACE('',(#947,#471),#608,.T.);
#6790=ADVANCED_FACE('',(#948,#472),#609,.T.);
#6791=ADVANCED_FACE('',(#949),#610,.T.);
#6792=ADVANCED_FACE('',(#950),#611,.F.);
#6793=ADVANCED_FACE('',(#951),#6617,.F.);
#6794=ADVANCED_FACE('',(#952),#612,.T.);
#6795=ADVANCED_FACE('',(#953,#473,#474),#613,.T.);
#6796=ADVANCED_FACE('',(#954),#6618,.F.);
#6797=ADVANCED_FACE('',(#955,#475),#614,.T.);
#6798=ADVANCED_FACE('',(#956),#6619,.F.);
#6799=ADVANCED_FACE('',(#957),#6620,.F.);
#6800=ADVANCED_FACE('',(#958,#476),#615,.T.);
#6801=ADVANCED_FACE('',(#959,#477),#616,.T.);
#6802=ADVANCED_FACE('',(#960),#617,.T.);
#6803=ADVANCED_FACE('',(#961),#618,.F.);
#6804=ADVANCED_FACE('',(#962),#619,.F.);
#6805=ADVANCED_FACE('',(#963),#620,.F.);
#6806=ADVANCED_FACE('',(#964),#621,.F.);
#6807=ADVANCED_FACE('',(#965),#622,.F.);
#6808=ADVANCED_FACE('',(#966),#623,.F.);
#6809=ADVANCED_FACE('',(#967),#624,.F.);
#6810=ADVANCED_FACE('',(#968),#625,.F.);
#6811=ADVANCED_FACE('',(#969),#626,.F.);
#6812=ADVANCED_FACE('',(#970),#627,.F.);
#6813=ADVANCED_FACE('',(#971),#628,.F.);
#6814=ADVANCED_FACE('',(#972),#629,.F.);
#6815=ADVANCED_FACE('',(#973),#630,.F.);
#6816=ADVANCED_FACE('',(#974),#631,.F.);
#6817=ADVANCED_FACE('',(#975),#632,.F.);
#6818=ADVANCED_FACE('',(#976),#633,.F.);
#6819=ADVANCED_FACE('',(#977),#634,.F.);
#6820=ADVANCED_FACE('',(#978),#635,.F.);
#6821=ADVANCED_FACE('',(#979),#636,.F.);
#6822=ADVANCED_FACE('',(#980),#637,.F.);
#6823=ADVANCED_FACE('',(#981),#638,.F.);
#6824=ADVANCED_FACE('',(#982),#639,.F.);
#6825=ADVANCED_FACE('',(#983),#640,.F.);
#6826=ADVANCED_FACE('',(#984),#641,.F.);
#6827=ADVANCED_FACE('',(#985),#642,.F.);
#6828=ADVANCED_FACE('',(#986),#643,.F.);
#6829=ADVANCED_FACE('',(#987),#644,.F.);
#6830=ADVANCED_FACE('',(#988),#645,.F.);
#6831=ADVANCED_FACE('',(#989),#646,.F.);
#6832=ADVANCED_FACE('',(#990),#647,.F.);
#6833=ADVANCED_FACE('',(#991),#648,.F.);
#6834=ADVANCED_FACE('',(#992),#649,.F.);
#6835=ADVANCED_FACE('',(#993),#650,.F.);
#6836=ADVANCED_FACE('',(#994),#651,.F.);
#6837=ADVANCED_FACE('',(#995),#652,.F.);
#6838=ADVANCED_FACE('',(#996),#653,.F.);
#6839=ADVANCED_FACE('',(#997),#654,.F.);
#6840=ADVANCED_FACE('',(#998),#6621,.F.);
#6841=ADVANCED_FACE('',(#999),#655,.T.);
#6842=ADVANCED_FACE('',(#1000),#656,.T.);
#6843=ADVANCED_FACE('',(#1001),#657,.T.);
#6844=ADVANCED_FACE('',(#1002),#658,.T.);
#6845=ADVANCED_FACE('',(#1003),#659,.T.);
#6846=ADVANCED_FACE('',(#1004),#660,.T.);
#6847=ADVANCED_FACE('',(#1005),#661,.T.);
#6848=ADVANCED_FACE('',(#1006),#662,.T.);
#6849=ADVANCED_FACE('',(#1007,#478),#663,.T.);
#6850=ADVANCED_FACE('',(#1008,#479),#664,.F.);
#6851=ADVANCED_FACE('',(#1009),#6622,.F.);
#6852=ADVANCED_FACE('',(#1010,#480),#665,.T.);
#6853=ADVANCED_FACE('',(#1011),#6623,.F.);
#6854=ADVANCED_FACE('',(#1012,#481),#666,.T.);
#6855=ADVANCED_FACE('',(#1013),#6624,.F.);
#6856=ADVANCED_FACE('',(#1014,#482),#667,.T.);
#6857=ADVANCED_FACE('',(#1015),#6625,.F.);
#6858=ADVANCED_FACE('',(#1016,#483),#668,.T.);
#6859=ADVANCED_FACE('',(#1017),#6626,.F.);
#6860=ADVANCED_FACE('',(#1018),#6627,.F.);
#6861=ADVANCED_FACE('',(#1019),#6628,.F.);
#6862=ADVANCED_FACE('',(#1020),#6629,.F.);
#6863=ADVANCED_FACE('',(#1021),#669,.T.);
#6864=ADVANCED_FACE('',(#1022),#670,.T.);
#6865=ADVANCED_FACE('',(#1023),#671,.T.);
#6866=ADVANCED_FACE('',(#1024),#672,.T.);
#6867=ADVANCED_FACE('',(#1025,#484,#485,#486,#487),#673,.T.);
#6868=ADVANCED_FACE('',(#1026),#674,.T.);
#6869=ADVANCED_FACE('',(#1027),#675,.T.);
#6870=ADVANCED_FACE('',(#1028),#676,.T.);
#6871=ADVANCED_FACE('',(#1029),#677,.T.);
#6872=ADVANCED_FACE('',(#1030),#678,.T.);
#6873=ADVANCED_FACE('',(#1031,#488,#489,#490,#491),#679,.T.);
#6874=ADVANCED_FACE('',(#1032),#680,.T.);
#6875=ADVANCED_FACE('',(#1033),#681,.T.);
#6876=ADVANCED_FACE('',(#1034),#682,.F.);
#6877=ADVANCED_FACE('',(#1035),#683,.F.);
#6878=ADVANCED_FACE('',(#1036),#684,.F.);
#6879=ADVANCED_FACE('',(#1037),#685,.F.);
#6880=ADVANCED_FACE('',(#1038),#686,.F.);
#6881=ADVANCED_FACE('',(#1039),#687,.F.);
#6882=ADVANCED_FACE('',(#1040),#688,.F.);
#6883=ADVANCED_FACE('',(#1041),#689,.F.);
#6884=ADVANCED_FACE('',(#1042),#690,.F.);
#6885=ADVANCED_FACE('',(#1043,#492),#691,.T.);
#6886=ADVANCED_FACE('',(#1044),#6630,.T.);
#6887=ADVANCED_FACE('',(#1045),#692,.F.);
#6888=ADVANCED_FACE('',(#1046),#693,.T.);
#6889=ADVANCED_FACE('',(#1047),#247,.T.);
#6890=ADVANCED_FACE('',(#1048),#6631,.T.);
#6891=ADVANCED_FACE('',(#1049),#248,.T.);
#6892=ADVANCED_FACE('',(#1050,#493),#694,.T.);
#6893=ADVANCED_FACE('',(#1051),#249,.T.);
#6894=ADVANCED_FACE('',(#1052),#6632,.T.);
#6895=ADVANCED_FACE('',(#1053),#695,.T.);
#6896=ADVANCED_FACE('',(#1054),#250,.T.);
#6897=ADVANCED_FACE('',(#1055),#6633,.T.);
#6898=ADVANCED_FACE('',(#1056),#251,.T.);
#6899=ADVANCED_FACE('',(#1057,#494),#696,.T.);
#6900=ADVANCED_FACE('',(#1058),#252,.T.);
#6901=ADVANCED_FACE('',(#1059),#6634,.T.);
#6902=ADVANCED_FACE('',(#1060),#253,.T.);
#6903=ADVANCED_FACE('',(#1061),#697,.T.);
#6904=ADVANCED_FACE('',(#1062),#698,.F.);
#6905=ADVANCED_FACE('',(#1063),#699,.F.);
#6906=ADVANCED_FACE('',(#1064),#700,.F.);
#6907=ADVANCED_FACE('',(#1065),#701,.F.);
#6908=ADVANCED_FACE('',(#1066),#702,.F.);
#6909=ADVANCED_FACE('',(#1067),#703,.F.);
#6910=ADVANCED_FACE('',(#1068),#704,.F.);
#6911=ADVANCED_FACE('',(#1069),#705,.F.);
#6912=ADVANCED_FACE('',(#1070),#706,.F.);
#6913=ADVANCED_FACE('',(#1071),#707,.T.);
#6914=ADVANCED_FACE('',(#1072,#495),#708,.T.);
#6915=ADVANCED_FACE('',(#1073),#709,.T.);
#6916=ADVANCED_FACE('',(#1074),#710,.T.);
#6917=ADVANCED_FACE('',(#1075),#711,.F.);
#6918=ADVANCED_FACE('',(#1076),#712,.T.);
#6919=ADVANCED_FACE('',(#1077),#713,.T.);
#6920=ADVANCED_FACE('',(#1078),#714,.T.);
#6921=ADVANCED_FACE('',(#1079),#6635,.F.);
#6922=ADVANCED_FACE('',(#1080),#715,.F.);
#6923=ADVANCED_FACE('',(#1081),#716,.F.);
#6924=ADVANCED_FACE('',(#1082),#717,.T.);
#6925=ADVANCED_FACE('',(#1083),#718,.T.);
#6926=ADVANCED_FACE('',(#1084),#254,.F.);
#6927=ADVANCED_FACE('',(#1085),#6636,.F.);
#6928=ADVANCED_FACE('',(#1086,#496),#719,.T.);
#6929=ADVANCED_FACE('',(#1087),#6637,.T.);
#6930=ADVANCED_FACE('',(#1088,#497),#720,.F.);
#6931=ADVANCED_FACE('',(#1089),#6638,.F.);
#6932=ADVANCED_FACE('',(#1090),#721,.F.);
#6933=ADVANCED_FACE('',(#1091),#722,.T.);
#6934=ADVANCED_FACE('',(#1092),#723,.T.);
#6935=ADVANCED_FACE('',(#1093),#724,.T.);
#6936=ADVANCED_FACE('',(#1094),#725,.T.);
#6937=ADVANCED_FACE('',(#1095),#6639,.F.);
#6938=ADVANCED_FACE('',(#1096),#6640,.F.);
#6939=ADVANCED_FACE('',(#1097),#6641,.F.);
#6940=ADVANCED_FACE('',(#1098),#6642,.F.);
#6941=ADVANCED_FACE('',(#1099),#726,.T.);
#6942=ADVANCED_FACE('',(#1100,#498,#499,#500,#501,#502),#727,.T.);
#6943=ADVANCED_FACE('',(#1101),#6643,.F.);
#6944=ADVANCED_FACE('',(#1102,#503,#504,#505),#728,.F.);
#6945=ADVANCED_FACE('',(#1103),#6644,.F.);
#6946=ADVANCED_FACE('',(#1104),#6645,.F.);
#6947=ADVANCED_FACE('',(#1105),#729,.T.);
#6948=ADVANCED_FACE('',(#1106),#6646,.F.);
#6949=ADVANCED_FACE('',(#1107),#6647,.F.);
#6950=ADVANCED_FACE('',(#1108),#730,.T.);
#6951=ADVANCED_FACE('',(#1109),#731,.T.);
#6952=ADVANCED_FACE('',(#1110),#732,.T.);
#6953=ADVANCED_FACE('',(#1111),#733,.T.);
#6954=ADVANCED_FACE('',(#1112),#734,.T.);
#6955=ADVANCED_FACE('',(#1113,#506,#507,#508),#735,.T.);
#6956=ADVANCED_FACE('',(#1114),#736,.T.);
#6957=ADVANCED_FACE('',(#1115,#509,#510,#511,#512,#513),#737,.T.);
#6958=ADVANCED_FACE('',(#1116),#738,.T.);
#6959=ADVANCED_FACE('',(#1117),#739,.T.);
#6960=ADVANCED_FACE('',(#1118),#740,.F.);
#6961=ADVANCED_FACE('',(#1119),#6648,.F.);
#6962=ADVANCED_FACE('',(#1120),#6649,.T.);
#6963=ADVANCED_FACE('',(#1121,#514),#741,.T.);
#6964=ADVANCED_FACE('',(#1122,#515),#742,.F.);
#6965=ADVANCED_FACE('',(#1123),#6650,.T.);
#6966=ADVANCED_FACE('',(#1124),#743,.T.);
#6967=ADVANCED_FACE('',(#1125),#6651,.T.);
#6968=ADVANCED_FACE('',(#1126),#744,.F.);
#6969=ADVANCED_FACE('',(#1127,#516),#745,.F.);
#6970=ADVANCED_FACE('',(#1128),#6652,.T.);
#6971=ADVANCED_FACE('',(#1129,#517),#746,.T.);
#6972=ADVANCED_FACE('',(#1130),#6653,.T.);
#6973=ADVANCED_FACE('',(#1131,#518),#747,.F.);
#6974=ADVANCED_FACE('',(#1132),#6654,.F.);
#6975=ADVANCED_FACE('',(#1133),#6655,.T.);
#6976=ADVANCED_FACE('',(#1134,#519),#748,.T.);
#6977=ADVANCED_FACE('',(#1135,#520),#749,.F.);
#6978=ADVANCED_FACE('',(#1136),#6656,.F.);
#6979=ADVANCED_FACE('',(#1137),#6657,.F.);
#6980=ADVANCED_FACE('',(#1138),#750,.F.);
#6981=ADVANCED_FACE('',(#1139,#521),#751,.T.);
#6982=ADVANCED_FACE('',(#1140),#752,.T.);
#6983=ADVANCED_FACE('',(#1141,#522),#753,.T.);
#6984=ADVANCED_FACE('',(#1142,#523),#754,.T.);
#6985=ADVANCED_FACE('',(#1143),#755,.T.);
#6986=ADVANCED_FACE('',(#1144),#756,.F.);
#6987=ADVANCED_FACE('',(#1145),#757,.T.);
#6988=ADVANCED_FACE('',(#1146),#758,.T.);
#6989=ADVANCED_FACE('',(#1147),#759,.T.);
#6990=ADVANCED_FACE('',(#1148),#760,.T.);
#6991=ADVANCED_FACE('',(#1149),#761,.T.);
#6992=ADVANCED_FACE('',(#1150),#762,.F.);
#6993=ADVANCED_FACE('',(#1151),#6658,.T.);
#6994=ADVANCED_FACE('',(#1152),#763,.T.);
#6995=ADVANCED_FACE('',(#1153,#524),#764,.F.);
#6996=ADVANCED_FACE('',(#1154),#6659,.T.);
#6997=ADVANCED_FACE('',(#1155),#765,.F.);
#6998=ADVANCED_FACE('',(#1156),#766,.T.);
#6999=ADVANCED_FACE('',(#1157),#6660,.F.);
#7000=ADVANCED_FACE('',(#1158),#767,.T.);
#7001=ADVANCED_FACE('',(#1159),#6661,.F.);
#7002=ADVANCED_FACE('',(#1160),#768,.T.);
#7003=ADVANCED_FACE('',(#1161),#6662,.F.);
#7004=ADVANCED_FACE('',(#1162),#769,.T.);
#7005=ADVANCED_FACE('',(#1163),#6663,.F.);
#7006=ADVANCED_FACE('',(#1164),#770,.T.);
#7007=ADVANCED_FACE('',(#1165),#771,.T.);
#7008=ADVANCED_FACE('',(#1166),#772,.T.);
#7009=ADVANCED_FACE('',(#1167),#773,.T.);
#7010=ADVANCED_FACE('',(#1168),#774,.T.);
#7011=ADVANCED_FACE('',(#1169,#525,#526,#527,#528),#775,.T.);
#7012=ADVANCED_FACE('',(#1170),#776,.T.);
#7013=ADVANCED_FACE('',(#1171),#777,.T.);
#7014=ADVANCED_FACE('',(#1172),#778,.T.);
#7015=ADVANCED_FACE('',(#1173),#779,.T.);
#7016=ADVANCED_FACE('',(#1174),#780,.T.);
#7017=ADVANCED_FACE('',(#1175),#781,.T.);
#7018=ADVANCED_FACE('',(#1176),#782,.T.);
#7019=ADVANCED_FACE('',(#1177),#783,.T.);
#7020=ADVANCED_FACE('',(#1178),#784,.T.);
#7021=ADVANCED_FACE('',(#1179),#785,.T.);
#7022=ADVANCED_FACE('',(#1180),#786,.T.);
#7023=ADVANCED_FACE('',(#1181),#787,.T.);
#7024=ADVANCED_FACE('',(#1182),#788,.T.);
#7025=ADVANCED_FACE('',(#1183),#789,.T.);
#7026=ADVANCED_FACE('',(#1184),#790,.T.);
#7027=ADVANCED_FACE('',(#1185),#791,.T.);
#7028=ADVANCED_FACE('',(#1186),#792,.T.);
#7029=ADVANCED_FACE('',(#1187),#793,.F.);
#7030=ADVANCED_FACE('',(#1188),#794,.T.);
#7031=ADVANCED_FACE('',(#1189),#795,.T.);
#7032=ADVANCED_FACE('',(#1190),#796,.T.);
#7033=ADVANCED_FACE('',(#1191),#797,.T.);
#7034=ADVANCED_FACE('',(#1192),#798,.T.);
#7035=ADVANCED_FACE('',(#1193),#799,.T.);
#7036=ADVANCED_FACE('',(#1194),#800,.T.);
#7037=ADVANCED_FACE('',(#1195),#801,.T.);
#7038=ADVANCED_FACE('',(#1196),#802,.T.);
#7039=ADVANCED_FACE('',(#1197),#803,.T.);
#7040=ADVANCED_FACE('',(#1198),#804,.F.);
#7041=ADVANCED_FACE('',(#1199),#805,.F.);
#7042=ADVANCED_FACE('',(#1200),#806,.F.);
#7043=ADVANCED_FACE('',(#1201),#807,.F.);
#7044=ADVANCED_FACE('',(#1202),#808,.F.);
#7045=ADVANCED_FACE('',(#1203),#809,.F.);
#7046=ADVANCED_FACE('',(#1204),#810,.F.);
#7047=ADVANCED_FACE('',(#1205),#811,.F.);
#7048=ADVANCED_FACE('',(#1206),#812,.F.);
#7049=ADVANCED_FACE('',(#1207),#813,.T.);
#7050=ADVANCED_FACE('',(#1208),#255,.T.);
#7051=ADVANCED_FACE('',(#1209),#6664,.T.);
#7052=ADVANCED_FACE('',(#1210),#256,.T.);
#7053=ADVANCED_FACE('',(#1211,#529),#814,.T.);
#7054=ADVANCED_FACE('',(#1212),#257,.T.);
#7055=ADVANCED_FACE('',(#1213),#6665,.T.);
#7056=ADVANCED_FACE('',(#1214),#815,.T.);
#7057=ADVANCED_FACE('',(#1215),#258,.T.);
#7058=ADVANCED_FACE('',(#1216),#6666,.T.);
#7059=ADVANCED_FACE('',(#1217),#259,.T.);
#7060=ADVANCED_FACE('',(#1218,#530),#816,.T.);
#7061=ADVANCED_FACE('',(#1219),#260,.T.);
#7062=ADVANCED_FACE('',(#1220),#6667,.T.);
#7063=ADVANCED_FACE('',(#1221),#261,.T.);
#7064=ADVANCED_FACE('',(#1222),#817,.T.);
#7065=ADVANCED_FACE('',(#1223),#818,.F.);
#7066=ADVANCED_FACE('',(#1224),#819,.F.);
#7067=ADVANCED_FACE('',(#1225),#820,.F.);
#7068=ADVANCED_FACE('',(#1226),#821,.F.);
#7069=ADVANCED_FACE('',(#1227),#822,.F.);
#7070=ADVANCED_FACE('',(#1228),#823,.F.);
#7071=ADVANCED_FACE('',(#1229),#824,.F.);
#7072=ADVANCED_FACE('',(#1230),#825,.F.);
#7073=CLOSED_SHELL('',(#6668,#6669,#6670,#6671,#6672,#6673,#6674,#6675,
#6676,#6677,#6678,#6679,#6680,#6681,#6682));
#7074=CLOSED_SHELL('',(#6683,#6684,#6685,#6686,#6687,#6688));
#7075=CLOSED_SHELL('',(#6689,#6690,#6691,#6692,#6693,#6694));
#7076=CLOSED_SHELL('',(#6695,#6696,#6697,#6698,#6699,#6700,#6701));
#7077=CLOSED_SHELL('',(#6702,#6703,#6704,#6705,#6706,#6707,#6708,#6709,
#6710,#6711,#6712,#6713,#6714,#6715,#6716,#6717,#6718,#6719));
#7078=CLOSED_SHELL('',(#6720,#6721,#6722,#6723,#6724,#6725,#6726));
#7079=CLOSED_SHELL('',(#6727,#6728,#6729,#6730,#6731,#6732,#6733));
#7080=CLOSED_SHELL('',(#6734,#6735,#6736,#6737,#6738,#6739,#6740,#6741,
#6742));
#7081=CLOSED_SHELL('',(#6743,#6744,#6745,#6746));
#7082=CLOSED_SHELL('',(#6747,#6748,#6749,#6750,#6751,#6752,#6753,#6754,
#6755,#6756));
#7083=CLOSED_SHELL('',(#6757,#6758,#6759,#6760,#6761,#6762,#6763));
#7084=CLOSED_SHELL('',(#6764,#6765,#6766,#6767));
#7085=CLOSED_SHELL('',(#6768,#6769,#6770,#6771,#6772,#6773,#6774));
#7086=CLOSED_SHELL('',(#6775,#6776,#6777,#6778));
#7087=CLOSED_SHELL('',(#6779,#6780,#6781));
#7088=CLOSED_SHELL('',(#6782,#6783,#6784,#6785,#6786,#6787,#6788,#6789,
#6790,#6791,#6792));
#7089=CLOSED_SHELL('',(#6793,#6794,#6795,#6796,#6797,#6798,#6799,#6800,
#6801,#6802,#6803));
#7090=CLOSED_SHELL('',(#6804,#6805,#6806,#6807,#6808,#6809,#6810,#6811,
#6812,#6813,#6814,#6815,#6816,#6817,#6818,#6819,#6820,#6821,#6822,#6823,
#6824,#6825,#6826,#6827,#6828,#6829,#6830,#6831,#6832,#6833,#6834,#6835,
#6836,#6837,#6838,#6839,#6840,#6841,#6842,#6843,#6844,#6845,#6846,#6847,
#6848,#6849,#6850));
#7091=CLOSED_SHELL('',(#6851,#6852,#6853,#6854,#6855,#6856,#6857,#6858,
#6859,#6860,#6861,#6862,#6863,#6864,#6865,#6866,#6867,#6868,#6869,#6870,
#6871,#6872,#6873,#6874,#6875,#6876));
#7092=CLOSED_SHELL('',(#6877,#6878,#6879,#6880,#6881,#6882,#6883,#6884));
#7093=CLOSED_SHELL('',(#6885,#6886,#6887,#6888,#6889,#6890,#6891,#6892,
#6893,#6894));
#7094=CLOSED_SHELL('',(#6895,#6896,#6897,#6898,#6899,#6900,#6901,#6902,
#6903));
#7095=CLOSED_SHELL('',(#6904,#6905,#6906,#6907,#6908,#6909,#6910,#6911));
#7096=CLOSED_SHELL('',(#6912,#6913,#6914,#6915,#6916,#6917,#6918,#6919,
#6920,#6921,#6922,#6923,#6924,#6925));
#7097=CLOSED_SHELL('',(#6926,#6927,#6928,#6929,#6930));
#7098=CLOSED_SHELL('',(#6931,#6932,#6933,#6934,#6935,#6936,#6937,#6938,
#6939,#6940,#6941,#6942,#6943,#6944,#6945,#6946,#6947,#6948,#6949,#6950,
#6951,#6952,#6953,#6954,#6955,#6956,#6957,#6958,#6959,#6960));
#7099=CLOSED_SHELL('',(#6961,#6962,#6963,#6964));
#7100=CLOSED_SHELL('',(#6965,#6966,#6967,#6968,#6969,#6970,#6971,#6972,
#6973));
#7101=CLOSED_SHELL('',(#6974,#6975,#6976,#6977));
#7102=CLOSED_SHELL('',(#6978,#6979,#6980,#6981,#6982,#6983,#6984,#6985,
#6986));
#7103=CLOSED_SHELL('',(#6987,#6988,#6989,#6990,#6991,#6992));
#7104=CLOSED_SHELL('',(#6993,#6994,#6995,#6996,#6997));
#7105=CLOSED_SHELL('',(#6998,#6999,#7000,#7001,#7002,#7003,#7004,#7005,
#7006,#7007,#7008,#7009,#7010,#7011,#7012,#7013,#7014,#7015,#7016,#7017,
#7018,#7019));
#7106=CLOSED_SHELL('',(#7020,#7021,#7022,#7023,#7024,#7025,#7026,#7027,
#7028,#7029));
#7107=CLOSED_SHELL('',(#7030,#7031,#7032,#7033,#7034,#7035,#7036,#7037,
#7038,#7039));
#7108=CLOSED_SHELL('',(#7040,#7041,#7042,#7043,#7044,#7045,#7046,#7047));
#7109=CLOSED_SHELL('',(#7048,#7049,#7050,#7051,#7052,#7053,#7054,#7055));
#7110=CLOSED_SHELL('',(#7056,#7057,#7058,#7059,#7060,#7061,#7062,#7063,
#7064));
#7111=CLOSED_SHELL('',(#7065,#7066,#7067,#7068,#7069,#7070,#7071,#7072));
#7112=DERIVED_UNIT_ELEMENT(#7182,1.);
#7113=DERIVED_UNIT_ELEMENT(#15042,-3.);
#7114=DERIVED_UNIT_ELEMENT(#7182,1.);
#7115=DERIVED_UNIT_ELEMENT(#15042,-3.);
#7116=DERIVED_UNIT_ELEMENT(#7182,1.);
#7117=DERIVED_UNIT_ELEMENT(#15042,-3.);
#7118=DERIVED_UNIT_ELEMENT(#7182,1.);
#7119=DERIVED_UNIT_ELEMENT(#15042,-3.);
#7120=DERIVED_UNIT_ELEMENT(#7182,1.);
#7121=DERIVED_UNIT_ELEMENT(#15042,-3.);
#7122=DERIVED_UNIT_ELEMENT(#7182,1.);
#7123=DERIVED_UNIT_ELEMENT(#15042,-3.);
#7124=DERIVED_UNIT_ELEMENT(#7182,1.);
#7125=DERIVED_UNIT_ELEMENT(#15042,-3.);
#7126=DERIVED_UNIT_ELEMENT(#7182,1.);
#7127=DERIVED_UNIT_ELEMENT(#15042,-3.);
#7128=DERIVED_UNIT_ELEMENT(#7182,1.);
#7129=DERIVED_UNIT_ELEMENT(#15042,-3.);
#7130=DERIVED_UNIT_ELEMENT(#7182,1.);
#7131=DERIVED_UNIT_ELEMENT(#15042,-3.);
#7132=DERIVED_UNIT_ELEMENT(#7182,1.);
#7133=DERIVED_UNIT_ELEMENT(#15042,-3.);
#7134=DERIVED_UNIT_ELEMENT(#7182,1.);
#7135=DERIVED_UNIT_ELEMENT(#15042,-3.);
#7136=DERIVED_UNIT_ELEMENT(#7182,1.);
#7137=DERIVED_UNIT_ELEMENT(#15042,-3.);
#7138=DERIVED_UNIT_ELEMENT(#7182,1.);
#7139=DERIVED_UNIT_ELEMENT(#15042,-3.);
#7140=DERIVED_UNIT_ELEMENT(#7182,1.);
#7141=DERIVED_UNIT_ELEMENT(#15042,-3.);
#7142=DERIVED_UNIT_ELEMENT(#7182,1.);
#7143=DERIVED_UNIT_ELEMENT(#15042,-3.);
#7144=DERIVED_UNIT_ELEMENT(#7182,1.);
#7145=DERIVED_UNIT_ELEMENT(#15042,-3.);
#7146=DERIVED_UNIT_ELEMENT(#7182,1.);
#7147=DERIVED_UNIT_ELEMENT(#15042,-3.);
#7148=DERIVED_UNIT_ELEMENT(#7182,1.);
#7149=DERIVED_UNIT_ELEMENT(#15042,-3.);
#7150=DERIVED_UNIT_ELEMENT(#7182,1.);
#7151=DERIVED_UNIT_ELEMENT(#15042,-3.);
#7152=DERIVED_UNIT_ELEMENT(#7182,1.);
#7153=DERIVED_UNIT_ELEMENT(#15042,-3.);
#7154=DERIVED_UNIT_ELEMENT(#7182,1.);
#7155=DERIVED_UNIT_ELEMENT(#15042,-3.);
#7156=DERIVED_UNIT_ELEMENT(#7182,1.);
#7157=DERIVED_UNIT_ELEMENT(#15042,-3.);
#7158=DERIVED_UNIT_ELEMENT(#7182,1.);
#7159=DERIVED_UNIT_ELEMENT(#15042,-3.);
#7160=DERIVED_UNIT_ELEMENT(#7182,1.);
#7161=DERIVED_UNIT_ELEMENT(#15042,-3.);
#7162=DERIVED_UNIT_ELEMENT(#7182,1.);
#7163=DERIVED_UNIT_ELEMENT(#15042,-3.);
#7164=DERIVED_UNIT_ELEMENT(#7182,1.);
#7165=DERIVED_UNIT_ELEMENT(#15042,-3.);
#7166=DERIVED_UNIT_ELEMENT(#7182,1.);
#7167=DERIVED_UNIT_ELEMENT(#15042,-3.);
#7168=DERIVED_UNIT_ELEMENT(#7182,1.);
#7169=DERIVED_UNIT_ELEMENT(#15042,-3.);
#7170=DERIVED_UNIT_ELEMENT(#7182,1.);
#7171=DERIVED_UNIT_ELEMENT(#15042,-3.);
#7172=DERIVED_UNIT_ELEMENT(#7182,1.);
#7173=DERIVED_UNIT_ELEMENT(#15042,-3.);
#7174=DERIVED_UNIT_ELEMENT(#7182,1.);
#7175=DERIVED_UNIT_ELEMENT(#15042,-3.);
#7176=DERIVED_UNIT_ELEMENT(#7182,1.);
#7177=DERIVED_UNIT_ELEMENT(#15042,-3.);
#7178=DERIVED_UNIT_ELEMENT(#7182,1.);
#7179=DERIVED_UNIT_ELEMENT(#15042,-3.);
#7180=DERIVED_UNIT_ELEMENT(#7182,1.);
#7181=DERIVED_UNIT_ELEMENT(#15042,-3.);
#7182=(
MASS_UNIT()
NAMED_UNIT(*)
SI_UNIT(.KILO.,.GRAM.)
);
#7183=DERIVED_UNIT((#7112,#7113));
#7184=DERIVED_UNIT((#7114,#7115));
#7185=DERIVED_UNIT((#7116,#7117));
#7186=DERIVED_UNIT((#7118,#7119));
#7187=DERIVED_UNIT((#7120,#7121));
#7188=DERIVED_UNIT((#7122,#7123));
#7189=DERIVED_UNIT((#7124,#7125));
#7190=DERIVED_UNIT((#7126,#7127));
#7191=DERIVED_UNIT((#7128,#7129));
#7192=DERIVED_UNIT((#7130,#7131));
#7193=DERIVED_UNIT((#7132,#7133));
#7194=DERIVED_UNIT((#7134,#7135));
#7195=DERIVED_UNIT((#7136,#7137));
#7196=DERIVED_UNIT((#7138,#7139));
#7197=DERIVED_UNIT((#7140,#7141));
#7198=DERIVED_UNIT((#7142,#7143));
#7199=DERIVED_UNIT((#7144,#7145));
#7200=DERIVED_UNIT((#7146,#7147));
#7201=DERIVED_UNIT((#7148,#7149));
#7202=DERIVED_UNIT((#7150,#7151));
#7203=DERIVED_UNIT((#7152,#7153));
#7204=DERIVED_UNIT((#7154,#7155));
#7205=DERIVED_UNIT((#7156,#7157));
#7206=DERIVED_UNIT((#7158,#7159));
#7207=DERIVED_UNIT((#7160,#7161));
#7208=DERIVED_UNIT((#7162,#7163));
#7209=DERIVED_UNIT((#7164,#7165));
#7210=DERIVED_UNIT((#7166,#7167));
#7211=DERIVED_UNIT((#7168,#7169));
#7212=DERIVED_UNIT((#7170,#7171));
#7213=DERIVED_UNIT((#7172,#7173));
#7214=DERIVED_UNIT((#7174,#7175));
#7215=DERIVED_UNIT((#7176,#7177));
#7216=DERIVED_UNIT((#7178,#7179));
#7217=DERIVED_UNIT((#7180,#7181));
#7218=MEASURE_REPRESENTATION_ITEM('density measure',
POSITIVE_RATIO_MEASURE(7850.),#7183);
#7219=MEASURE_REPRESENTATION_ITEM('density measure',
POSITIVE_RATIO_MEASURE(7850.),#7184);
#7220=MEASURE_REPRESENTATION_ITEM('density measure',
POSITIVE_RATIO_MEASURE(7850.),#7185);
#7221=MEASURE_REPRESENTATION_ITEM('density measure',
POSITIVE_RATIO_MEASURE(7850.),#7186);
#7222=MEASURE_REPRESENTATION_ITEM('density measure',
POSITIVE_RATIO_MEASURE(7850.),#7187);
#7223=MEASURE_REPRESENTATION_ITEM('density measure',
POSITIVE_RATIO_MEASURE(7850.),#7188);
#7224=MEASURE_REPRESENTATION_ITEM('density measure',
POSITIVE_RATIO_MEASURE(7850.),#7189);
#7225=MEASURE_REPRESENTATION_ITEM('density measure',
POSITIVE_RATIO_MEASURE(7850.),#7190);
#7226=MEASURE_REPRESENTATION_ITEM('density measure',
POSITIVE_RATIO_MEASURE(7850.),#7191);
#7227=MEASURE_REPRESENTATION_ITEM('density measure',
POSITIVE_RATIO_MEASURE(7850.),#7192);
#7228=MEASURE_REPRESENTATION_ITEM('density measure',
POSITIVE_RATIO_MEASURE(7850.),#7193);
#7229=MEASURE_REPRESENTATION_ITEM('density measure',
POSITIVE_RATIO_MEASURE(7850.),#7194);
#7230=MEASURE_REPRESENTATION_ITEM('density measure',
POSITIVE_RATIO_MEASURE(7850.),#7195);
#7231=MEASURE_REPRESENTATION_ITEM('density measure',
POSITIVE_RATIO_MEASURE(7850.),#7196);
#7232=MEASURE_REPRESENTATION_ITEM('density measure',
POSITIVE_RATIO_MEASURE(7850.),#7197);
#7233=MEASURE_REPRESENTATION_ITEM('density measure',
POSITIVE_RATIO_MEASURE(7850.),#7198);
#7234=MEASURE_REPRESENTATION_ITEM('density measure',
POSITIVE_RATIO_MEASURE(7850.),#7199);
#7235=MEASURE_REPRESENTATION_ITEM('density measure',
POSITIVE_RATIO_MEASURE(7850.),#7200);
#7236=MEASURE_REPRESENTATION_ITEM('density measure',
POSITIVE_RATIO_MEASURE(7850.),#7201);
#7237=MEASURE_REPRESENTATION_ITEM('density measure',
POSITIVE_RATIO_MEASURE(7850.),#7202);
#7238=MEASURE_REPRESENTATION_ITEM('density measure',
POSITIVE_RATIO_MEASURE(7850.),#7203);
#7239=MEASURE_REPRESENTATION_ITEM('density measure',
POSITIVE_RATIO_MEASURE(7850.),#7204);
#7240=MEASURE_REPRESENTATION_ITEM('density measure',
POSITIVE_RATIO_MEASURE(7850.),#7205);
#7241=MEASURE_REPRESENTATION_ITEM('density measure',
POSITIVE_RATIO_MEASURE(7850.),#7206);
#7242=MEASURE_REPRESENTATION_ITEM('density measure',
POSITIVE_RATIO_MEASURE(7850.),#7207);
#7243=MEASURE_REPRESENTATION_ITEM('density measure',
POSITIVE_RATIO_MEASURE(7850.),#7208);
#7244=MEASURE_REPRESENTATION_ITEM('density measure',
POSITIVE_RATIO_MEASURE(7850.),#7209);
#7245=MEASURE_REPRESENTATION_ITEM('density measure',
POSITIVE_RATIO_MEASURE(7850.),#7210);
#7246=MEASURE_REPRESENTATION_ITEM('density measure',
POSITIVE_RATIO_MEASURE(7850.),#7211);
#7247=MEASURE_REPRESENTATION_ITEM('density measure',
POSITIVE_RATIO_MEASURE(7850.),#7212);
#7248=MEASURE_REPRESENTATION_ITEM('density measure',
POSITIVE_RATIO_MEASURE(7850.),#7213);
#7249=MEASURE_REPRESENTATION_ITEM('density measure',
POSITIVE_RATIO_MEASURE(7850.),#7214);
#7250=MEASURE_REPRESENTATION_ITEM('density measure',
POSITIVE_RATIO_MEASURE(7850.),#7215);
#7251=MEASURE_REPRESENTATION_ITEM('density measure',
POSITIVE_RATIO_MEASURE(7850.),#7216);
#7252=MEASURE_REPRESENTATION_ITEM('density measure',
POSITIVE_RATIO_MEASURE(7850.),#7217);
#7253=PROPERTY_DEFINITION_REPRESENTATION(#7428,#7323);
#7254=PROPERTY_DEFINITION_REPRESENTATION(#7429,#7324);
#7255=PROPERTY_DEFINITION_REPRESENTATION(#7430,#7325);
#7256=PROPERTY_DEFINITION_REPRESENTATION(#7431,#7326);
#7257=PROPERTY_DEFINITION_REPRESENTATION(#7432,#7327);
#7258=PROPERTY_DEFINITION_REPRESENTATION(#7433,#7328);
#7259=PROPERTY_DEFINITION_REPRESENTATION(#7434,#7329);
#7260=PROPERTY_DEFINITION_REPRESENTATION(#7435,#7330);
#7261=PROPERTY_DEFINITION_REPRESENTATION(#7436,#7331);
#7262=PROPERTY_DEFINITION_REPRESENTATION(#7437,#7332);
#7263=PROPERTY_DEFINITION_REPRESENTATION(#7438,#7333);
#7264=PROPERTY_DEFINITION_REPRESENTATION(#7439,#7334);
#7265=PROPERTY_DEFINITION_REPRESENTATION(#7440,#7335);
#7266=PROPERTY_DEFINITION_REPRESENTATION(#7441,#7336);
#7267=PROPERTY_DEFINITION_REPRESENTATION(#7442,#7337);
#7268=PROPERTY_DEFINITION_REPRESENTATION(#7443,#7338);
#7269=PROPERTY_DEFINITION_REPRESENTATION(#7444,#7339);
#7270=PROPERTY_DEFINITION_REPRESENTATION(#7445,#7340);
#7271=PROPERTY_DEFINITION_REPRESENTATION(#7446,#7341);
#7272=PROPERTY_DEFINITION_REPRESENTATION(#7447,#7342);
#7273=PROPERTY_DEFINITION_REPRESENTATION(#7448,#7343);
#7274=PROPERTY_DEFINITION_REPRESENTATION(#7449,#7344);
#7275=PROPERTY_DEFINITION_REPRESENTATION(#7450,#7345);
#7276=PROPERTY_DEFINITION_REPRESENTATION(#7451,#7346);
#7277=PROPERTY_DEFINITION_REPRESENTATION(#7452,#7347);
#7278=PROPERTY_DEFINITION_REPRESENTATION(#7453,#7348);
#7279=PROPERTY_DEFINITION_REPRESENTATION(#7454,#7349);
#7280=PROPERTY_DEFINITION_REPRESENTATION(#7455,#7350);
#7281=PROPERTY_DEFINITION_REPRESENTATION(#7456,#7351);
#7282=PROPERTY_DEFINITION_REPRESENTATION(#7457,#7352);
#7283=PROPERTY_DEFINITION_REPRESENTATION(#7458,#7353);
#7284=PROPERTY_DEFINITION_REPRESENTATION(#7459,#7354);
#7285=PROPERTY_DEFINITION_REPRESENTATION(#7460,#7355);
#7286=PROPERTY_DEFINITION_REPRESENTATION(#7461,#7356);
#7287=PROPERTY_DEFINITION_REPRESENTATION(#7462,#7357);
#7288=PROPERTY_DEFINITION_REPRESENTATION(#7463,#7358);
#7289=PROPERTY_DEFINITION_REPRESENTATION(#7464,#7359);
#7290=PROPERTY_DEFINITION_REPRESENTATION(#7465,#7360);
#7291=PROPERTY_DEFINITION_REPRESENTATION(#7466,#7361);
#7292=PROPERTY_DEFINITION_REPRESENTATION(#7467,#7362);
#7293=PROPERTY_DEFINITION_REPRESENTATION(#7468,#7363);
#7294=PROPERTY_DEFINITION_REPRESENTATION(#7469,#7364);
#7295=PROPERTY_DEFINITION_REPRESENTATION(#7470,#7365);
#7296=PROPERTY_DEFINITION_REPRESENTATION(#7471,#7366);
#7297=PROPERTY_DEFINITION_REPRESENTATION(#7472,#7367);
#7298=PROPERTY_DEFINITION_REPRESENTATION(#7473,#7368);
#7299=PROPERTY_DEFINITION_REPRESENTATION(#7474,#7369);
#7300=PROPERTY_DEFINITION_REPRESENTATION(#7475,#7370);
#7301=PROPERTY_DEFINITION_REPRESENTATION(#7476,#7371);
#7302=PROPERTY_DEFINITION_REPRESENTATION(#7477,#7372);
#7303=PROPERTY_DEFINITION_REPRESENTATION(#7478,#7373);
#7304=PROPERTY_DEFINITION_REPRESENTATION(#7479,#7374);
#7305=PROPERTY_DEFINITION_REPRESENTATION(#7480,#7375);
#7306=PROPERTY_DEFINITION_REPRESENTATION(#7481,#7376);
#7307=PROPERTY_DEFINITION_REPRESENTATION(#7482,#7377);
#7308=PROPERTY_DEFINITION_REPRESENTATION(#7483,#7378);
#7309=PROPERTY_DEFINITION_REPRESENTATION(#7484,#7379);
#7310=PROPERTY_DEFINITION_REPRESENTATION(#7485,#7380);
#7311=PROPERTY_DEFINITION_REPRESENTATION(#7486,#7381);
#7312=PROPERTY_DEFINITION_REPRESENTATION(#7487,#7382);
#7313=PROPERTY_DEFINITION_REPRESENTATION(#7488,#7383);
#7314=PROPERTY_DEFINITION_REPRESENTATION(#7489,#7384);
#7315=PROPERTY_DEFINITION_REPRESENTATION(#7490,#7385);
#7316=PROPERTY_DEFINITION_REPRESENTATION(#7491,#7386);
#7317=PROPERTY_DEFINITION_REPRESENTATION(#7492,#7387);
#7318=PROPERTY_DEFINITION_REPRESENTATION(#7493,#7388);
#7319=PROPERTY_DEFINITION_REPRESENTATION(#7494,#7389);
#7320=PROPERTY_DEFINITION_REPRESENTATION(#7495,#7390);
#7321=PROPERTY_DEFINITION_REPRESENTATION(#7496,#7391);
#7322=PROPERTY_DEFINITION_REPRESENTATION(#7497,#7392);
#7323=REPRESENTATION('material name',(#7393),#15003);
#7324=REPRESENTATION('density',(#7218),#15003);
#7325=REPRESENTATION('material name',(#7394),#15004);
#7326=REPRESENTATION('density',(#7219),#15004);
#7327=REPRESENTATION('material name',(#7395),#15005);
#7328=REPRESENTATION('density',(#7220),#15005);
#7329=REPRESENTATION('material name',(#7396),#15006);
#7330=REPRESENTATION('density',(#7221),#15006);
#7331=REPRESENTATION('material name',(#7397),#15007);
#7332=REPRESENTATION('density',(#7222),#15007);
#7333=REPRESENTATION('material name',(#7398),#15008);
#7334=REPRESENTATION('density',(#7223),#15008);
#7335=REPRESENTATION('material name',(#7399),#15009);
#7336=REPRESENTATION('density',(#7224),#15009);
#7337=REPRESENTATION('material name',(#7400),#15010);
#7338=REPRESENTATION('density',(#7225),#15010);
#7339=REPRESENTATION('material name',(#7401),#15011);
#7340=REPRESENTATION('density',(#7226),#15011);
#7341=REPRESENTATION('material name',(#7402),#15012);
#7342=REPRESENTATION('density',(#7227),#15012);
#7343=REPRESENTATION('material name',(#7403),#15013);
#7344=REPRESENTATION('density',(#7228),#15013);
#7345=REPRESENTATION('material name',(#7404),#15014);
#7346=REPRESENTATION('density',(#7229),#15014);
#7347=REPRESENTATION('material name',(#7405),#15015);
#7348=REPRESENTATION('density',(#7230),#15015);
#7349=REPRESENTATION('material name',(#7406),#15016);
#7350=REPRESENTATION('density',(#7231),#15016);
#7351=REPRESENTATION('material name',(#7407),#15017);
#7352=REPRESENTATION('density',(#7232),#15017);
#7353=REPRESENTATION('material name',(#7408),#15018);
#7354=REPRESENTATION('density',(#7233),#15018);
#7355=REPRESENTATION('material name',(#7409),#15019);
#7356=REPRESENTATION('density',(#7234),#15019);
#7357=REPRESENTATION('material name',(#7410),#15020);
#7358=REPRESENTATION('density',(#7235),#15020);
#7359=REPRESENTATION('material name',(#7411),#15021);
#7360=REPRESENTATION('density',(#7236),#15021);
#7361=REPRESENTATION('material name',(#7412),#15022);
#7362=REPRESENTATION('density',(#7237),#15022);
#7363=REPRESENTATION('material name',(#7413),#15023);
#7364=REPRESENTATION('density',(#7238),#15023);
#7365=REPRESENTATION('material name',(#7414),#15024);
#7366=REPRESENTATION('density',(#7239),#15024);
#7367=REPRESENTATION('material name',(#7415),#15025);
#7368=REPRESENTATION('density',(#7240),#15025);
#7369=REPRESENTATION('material name',(#7416),#15027);
#7370=REPRESENTATION('density',(#7241),#15027);
#7371=REPRESENTATION('material name',(#7417),#15028);
#7372=REPRESENTATION('density',(#7242),#15028);
#7373=REPRESENTATION('material name',(#7418),#15029);
#7374=REPRESENTATION('density',(#7243),#15029);
#7375=REPRESENTATION('material name',(#7419),#15030);
#7376=REPRESENTATION('density',(#7244),#15030);
#7377=REPRESENTATION('material name',(#7420),#15031);
#7378=REPRESENTATION('density',(#7245),#15031);
#7379=REPRESENTATION('material name',(#7421),#15032);
#7380=REPRESENTATION('density',(#7246),#15032);
#7381=REPRESENTATION('material name',(#7422),#15033);
#7382=REPRESENTATION('density',(#7247),#15033);
#7383=REPRESENTATION('material name',(#7423),#15035);
#7384=REPRESENTATION('density',(#7248),#15035);
#7385=REPRESENTATION('material name',(#7424),#15036);
#7386=REPRESENTATION('density',(#7249),#15036);
#7387=REPRESENTATION('material name',(#7425),#15037);
#7388=REPRESENTATION('density',(#7250),#15037);
#7389=REPRESENTATION('material name',(#7426),#15038);
#7390=REPRESENTATION('density',(#7251),#15038);
#7391=REPRESENTATION('material name',(#7427),#15039);
#7392=REPRESENTATION('density',(#7252),#15039);
#7393=DESCRIPTIVE_REPRESENTATION_ITEM('Steel','Steel');
#7394=DESCRIPTIVE_REPRESENTATION_ITEM('Steel','Steel');
#7395=DESCRIPTIVE_REPRESENTATION_ITEM('Steel','Steel');
#7396=DESCRIPTIVE_REPRESENTATION_ITEM('Steel','Steel');
#7397=DESCRIPTIVE_REPRESENTATION_ITEM('Steel','Steel');
#7398=DESCRIPTIVE_REPRESENTATION_ITEM('Steel','Steel');
#7399=DESCRIPTIVE_REPRESENTATION_ITEM('Steel','Steel');
#7400=DESCRIPTIVE_REPRESENTATION_ITEM('Steel','Steel');
#7401=DESCRIPTIVE_REPRESENTATION_ITEM('Steel','Steel');
#7402=DESCRIPTIVE_REPRESENTATION_ITEM('Steel','Steel');
#7403=DESCRIPTIVE_REPRESENTATION_ITEM('Steel','Steel');
#7404=DESCRIPTIVE_REPRESENTATION_ITEM('Steel','Steel');
#7405=DESCRIPTIVE_REPRESENTATION_ITEM('Steel','Steel');
#7406=DESCRIPTIVE_REPRESENTATION_ITEM('Steel','Steel');
#7407=DESCRIPTIVE_REPRESENTATION_ITEM('Steel','Steel');
#7408=DESCRIPTIVE_REPRESENTATION_ITEM('Steel','Steel');
#7409=DESCRIPTIVE_REPRESENTATION_ITEM('Steel','Steel');
#7410=DESCRIPTIVE_REPRESENTATION_ITEM('Steel','Steel');
#7411=DESCRIPTIVE_REPRESENTATION_ITEM('Steel','Steel');
#7412=DESCRIPTIVE_REPRESENTATION_ITEM('Steel','Steel');
#7413=DESCRIPTIVE_REPRESENTATION_ITEM('Steel','Steel');
#7414=DESCRIPTIVE_REPRESENTATION_ITEM('Steel','Steel');
#7415=DESCRIPTIVE_REPRESENTATION_ITEM('Steel','Steel');
#7416=DESCRIPTIVE_REPRESENTATION_ITEM('Steel','Steel');
#7417=DESCRIPTIVE_REPRESENTATION_ITEM('Steel','Steel');
#7418=DESCRIPTIVE_REPRESENTATION_ITEM('Steel','Steel');
#7419=DESCRIPTIVE_REPRESENTATION_ITEM('Steel','Steel');
#7420=DESCRIPTIVE_REPRESENTATION_ITEM('Steel','Steel');
#7421=DESCRIPTIVE_REPRESENTATION_ITEM('Steel','Steel');
#7422=DESCRIPTIVE_REPRESENTATION_ITEM('Steel','Steel');
#7423=DESCRIPTIVE_REPRESENTATION_ITEM('Steel','Steel');
#7424=DESCRIPTIVE_REPRESENTATION_ITEM('Steel','Steel');
#7425=DESCRIPTIVE_REPRESENTATION_ITEM('Steel','Steel');
#7426=DESCRIPTIVE_REPRESENTATION_ITEM('Steel','Steel');
#7427=DESCRIPTIVE_REPRESENTATION_ITEM('Steel','Steel');
#7428=PROPERTY_DEFINITION('material property','material name',#15224);
#7429=PROPERTY_DEFINITION('material property','density of part',#15224);
#7430=PROPERTY_DEFINITION('material property','material name',#15225);
#7431=PROPERTY_DEFINITION('material property','density of part',#15225);
#7432=PROPERTY_DEFINITION('material property','material name',#15226);
#7433=PROPERTY_DEFINITION('material property','density of part',#15226);
#7434=PROPERTY_DEFINITION('material property','material name',#15227);
#7435=PROPERTY_DEFINITION('material property','density of part',#15227);
#7436=PROPERTY_DEFINITION('material property','material name',#15228);
#7437=PROPERTY_DEFINITION('material property','density of part',#15228);
#7438=PROPERTY_DEFINITION('material property','material name',#15229);
#7439=PROPERTY_DEFINITION('material property','density of part',#15229);
#7440=PROPERTY_DEFINITION('material property','material name',#15230);
#7441=PROPERTY_DEFINITION('material property','density of part',#15230);
#7442=PROPERTY_DEFINITION('material property','material name',#15231);
#7443=PROPERTY_DEFINITION('material property','density of part',#15231);
#7444=PROPERTY_DEFINITION('material property','material name',#15232);
#7445=PROPERTY_DEFINITION('material property','density of part',#15232);
#7446=PROPERTY_DEFINITION('material property','material name',#15233);
#7447=PROPERTY_DEFINITION('material property','density of part',#15233);
#7448=PROPERTY_DEFINITION('material property','material name',#15234);
#7449=PROPERTY_DEFINITION('material property','density of part',#15234);
#7450=PROPERTY_DEFINITION('material property','material name',#15235);
#7451=PROPERTY_DEFINITION('material property','density of part',#15235);
#7452=PROPERTY_DEFINITION('material property','material name',#15236);
#7453=PROPERTY_DEFINITION('material property','density of part',#15236);
#7454=PROPERTY_DEFINITION('material property','material name',#15237);
#7455=PROPERTY_DEFINITION('material property','density of part',#15237);
#7456=PROPERTY_DEFINITION('material property','material name',#15238);
#7457=PROPERTY_DEFINITION('material property','density of part',#15238);
#7458=PROPERTY_DEFINITION('material property','material name',#15239);
#7459=PROPERTY_DEFINITION('material property','density of part',#15239);
#7460=PROPERTY_DEFINITION('material property','material name',#15240);
#7461=PROPERTY_DEFINITION('material property','density of part',#15240);
#7462=PROPERTY_DEFINITION('material property','material name',#15241);
#7463=PROPERTY_DEFINITION('material property','density of part',#15241);
#7464=PROPERTY_DEFINITION('material property','material name',#15242);
#7465=PROPERTY_DEFINITION('material property','density of part',#15242);
#7466=PROPERTY_DEFINITION('material property','material name',#15243);
#7467=PROPERTY_DEFINITION('material property','density of part',#15243);
#7468=PROPERTY_DEFINITION('material property','material name',#15244);
#7469=PROPERTY_DEFINITION('material property','density of part',#15244);
#7470=PROPERTY_DEFINITION('material property','material name',#15245);
#7471=PROPERTY_DEFINITION('material property','density of part',#15245);
#7472=PROPERTY_DEFINITION('material property','material name',#15246);
#7473=PROPERTY_DEFINITION('material property','density of part',#15246);
#7474=PROPERTY_DEFINITION('material property','material name',#15248);
#7475=PROPERTY_DEFINITION('material property','density of part',#15248);
#7476=PROPERTY_DEFINITION('material property','material name',#15249);
#7477=PROPERTY_DEFINITION('material property','density of part',#15249);
#7478=PROPERTY_DEFINITION('material property','material name',#15250);
#7479=PROPERTY_DEFINITION('material property','density of part',#15250);
#7480=PROPERTY_DEFINITION('material property','material name',#15251);
#7481=PROPERTY_DEFINITION('material property','density of part',#15251);
#7482=PROPERTY_DEFINITION('material property','material name',#15252);
#7483=PROPERTY_DEFINITION('material property','density of part',#15252);
#7484=PROPERTY_DEFINITION('material property','material name',#15253);
#7485=PROPERTY_DEFINITION('material property','density of part',#15253);
#7486=PROPERTY_DEFINITION('material property','material name',#15254);
#7487=PROPERTY_DEFINITION('material property','density of part',#15254);
#7488=PROPERTY_DEFINITION('material property','material name',#15256);
#7489=PROPERTY_DEFINITION('material property','density of part',#15256);
#7490=PROPERTY_DEFINITION('material property','material name',#15257);
#7491=PROPERTY_DEFINITION('material property','density of part',#15257);
#7492=PROPERTY_DEFINITION('material property','material name',#15258);
#7493=PROPERTY_DEFINITION('material property','density of part',#15258);
#7494=PROPERTY_DEFINITION('material property','material name',#15259);
#7495=PROPERTY_DEFINITION('material property','density of part',#15259);
#7496=PROPERTY_DEFINITION('material property','material name',#15260);
#7497=PROPERTY_DEFINITION('material property','density of part',#15260);
#7498=AXIS2_PLACEMENT_3D('',#10338,#8221,#8222);
#7499=AXIS2_PLACEMENT_3D('',#10339,#8223,#8224);
#7500=AXIS2_PLACEMENT_3D('',#10340,#8225,#8226);
#7501=AXIS2_PLACEMENT_3D('',#10341,#8227,#8228);
#7502=AXIS2_PLACEMENT_3D('',#10343,#8229,#8230);
#7503=AXIS2_PLACEMENT_3D('',#10346,#8232,#8233);
#7504=AXIS2_PLACEMENT_3D('',#10347,#8234,#8235);
#7505=AXIS2_PLACEMENT_3D('',#10348,#8236,#8237);
#7506=AXIS2_PLACEMENT_3D('',#10350,#8238,#8239);
#7507=AXIS2_PLACEMENT_3D('',#10353,#8241,#8242);
#7508=AXIS2_PLACEMENT_3D('',#10354,#8243,#8244);
#7509=AXIS2_PLACEMENT_3D('',#10355,#8245,#8246);
#7510=AXIS2_PLACEMENT_3D('',#10357,#8247,#8248);
#7511=AXIS2_PLACEMENT_3D('',#10360,#8250,#8251);
#7512=AXIS2_PLACEMENT_3D('',#10361,#8252,#8253);
#7513=AXIS2_PLACEMENT_3D('',#10362,#8254,#8255);
#7514=AXIS2_PLACEMENT_3D('',#10364,#8256,#8257);
#7515=AXIS2_PLACEMENT_3D('',#10367,#8259,#8260);
#7516=AXIS2_PLACEMENT_3D('',#10368,#8261,#8262);
#7517=AXIS2_PLACEMENT_3D('',#10369,#8263,#8264);
#7518=AXIS2_PLACEMENT_3D('',#10371,#8265,#8266);
#7519=AXIS2_PLACEMENT_3D('',#10374,#8268,#8269);
#7520=AXIS2_PLACEMENT_3D('',#10375,#8270,#8271);
#7521=AXIS2_PLACEMENT_3D('',#10384,#8276,#8277);
#7522=AXIS2_PLACEMENT_3D('',#10390,#8281,#8282);
#7523=AXIS2_PLACEMENT_3D('',#10396,#8286,#8287);
#7524=AXIS2_PLACEMENT_3D('',#10399,#8290,#8291);
#7525=AXIS2_PLACEMENT_3D('',#10400,#8292,#8293);
#7526=AXIS2_PLACEMENT_3D('',#10401,#8294,#8295);
#7527=AXIS2_PLACEMENT_3D('',#10402,#8296,#8297);
#7528=AXIS2_PLACEMENT_3D('',#10411,#8302,#8303);
#7529=AXIS2_PLACEMENT_3D('',#10417,#8307,#8308);
#7530=AXIS2_PLACEMENT_3D('',#10423,#8312,#8313);
#7531=AXIS2_PLACEMENT_3D('',#10426,#8316,#8317);
#7532=AXIS2_PLACEMENT_3D('',#10427,#8318,#8319);
#7533=AXIS2_PLACEMENT_3D('',#10428,#8320,#8321);
#7534=AXIS2_PLACEMENT_3D('',#10429,#8322,#8323);
#7535=AXIS2_PLACEMENT_3D('',#10438,#8328,#8329);
#7536=AXIS2_PLACEMENT_3D('',#10444,#8333,#8334);
#7537=AXIS2_PLACEMENT_3D('',#10450,#8338,#8339);
#7538=AXIS2_PLACEMENT_3D('',#10453,#8342,#8343);
#7539=AXIS2_PLACEMENT_3D('',#10454,#8344,#8345);
#7540=AXIS2_PLACEMENT_3D('',#10455,#8346,#8347);
#7541=AXIS2_PLACEMENT_3D('',#10456,#8348,#8349);
#7542=AXIS2_PLACEMENT_3D('',#10458,#8350,#8351);
#7543=AXIS2_PLACEMENT_3D('',#10461,#8353,#8354);
#7544=AXIS2_PLACEMENT_3D('',#10462,#8355,#8356);
#7545=AXIS2_PLACEMENT_3D('',#10471,#8361,#8362);
#7546=AXIS2_PLACEMENT_3D('',#10477,#8366,#8367);
#7547=AXIS2_PLACEMENT_3D('',#10483,#8371,#8372);
#7548=AXIS2_PLACEMENT_3D('',#10486,#8375,#8376);
#7549=AXIS2_PLACEMENT_3D('',#10487,#8377,#8378);
#7550=AXIS2_PLACEMENT_3D('',#10488,#8379,#8380);
#7551=AXIS2_PLACEMENT_3D('',#10489,#8381,#8382);
#7552=AXIS2_PLACEMENT_3D('',#10491,#8383,#8384);
#7553=AXIS2_PLACEMENT_3D('',#10494,#8386,#8387);
#7554=AXIS2_PLACEMENT_3D('',#10495,#8388,#8389);
#7555=AXIS2_PLACEMENT_3D('',#10497,#8390,#8391);
#7556=AXIS2_PLACEMENT_3D('',#10500,#8393,#8394);
#7557=AXIS2_PLACEMENT_3D('',#10501,#8395,#8396);
#7558=AXIS2_PLACEMENT_3D('',#10503,#8397,#8398);
#7559=AXIS2_PLACEMENT_3D('',#10506,#8400,#8401);
#7560=AXIS2_PLACEMENT_3D('',#10507,#8402,#8403);
#7561=AXIS2_PLACEMENT_3D('',#10509,#8404,#8405);
#7562=AXIS2_PLACEMENT_3D('',#10512,#8407,#8408);
#7563=AXIS2_PLACEMENT_3D('',#10513,#8409,#8410);
#7564=AXIS2_PLACEMENT_3D('',#10515,#8411,#8412);
#7565=AXIS2_PLACEMENT_3D('',#10518,#8414,#8415);
#7566=AXIS2_PLACEMENT_3D('',#10519,#8416,#8417);
#7567=AXIS2_PLACEMENT_3D('',#10521,#8418,#8419);
#7568=AXIS2_PLACEMENT_3D('',#10524,#8421,#8422);
#7569=AXIS2_PLACEMENT_3D('',#10525,#8423,#8424);
#7570=AXIS2_PLACEMENT_3D('',#10527,#8425,#8426);
#7571=AXIS2_PLACEMENT_3D('',#10530,#8428,#8429);
#7572=AXIS2_PLACEMENT_3D('',#10531,#8430,#8431);
#7573=AXIS2_PLACEMENT_3D('',#10533,#8432,#8433);
#7574=AXIS2_PLACEMENT_3D('',#10536,#8435,#8436);
#7575=AXIS2_PLACEMENT_3D('',#10537,#8437,#8438);
#7576=AXIS2_PLACEMENT_3D('',#10546,#8443,#8444);
#7577=AXIS2_PLACEMENT_3D('',#10555,#8449,#8450);
#7578=AXIS2_PLACEMENT_3D('',#10558,#8453,#8454);
#7579=AXIS2_PLACEMENT_3D('',#10568,#8460,#8461);
#7580=AXIS2_PLACEMENT_3D('',#10572,#8464,#8465);
#7581=AXIS2_PLACEMENT_3D('',#10576,#8468,#8469);
#7582=AXIS2_PLACEMENT_3D('',#10582,#8473,#8474);
#7583=AXIS2_PLACEMENT_3D('',#10585,#8477,#8478);
#7584=AXIS2_PLACEMENT_3D('',#10586,#8479,#8480);
#7585=AXIS2_PLACEMENT_3D('',#10587,#8481,#8482);
#7586=AXIS2_PLACEMENT_3D('',#10588,#8483,#8484);
#7587=AXIS2_PLACEMENT_3D('',#10590,#8485,#8486);
#7588=AXIS2_PLACEMENT_3D('',#10593,#8488,#8489);
#7589=AXIS2_PLACEMENT_3D('',#10594,#8490,#8491);
#7590=AXIS2_PLACEMENT_3D('',#10603,#8496,#8497);
#7591=AXIS2_PLACEMENT_3D('',#10609,#8501,#8502);
#7592=AXIS2_PLACEMENT_3D('',#10615,#8506,#8507);
#7593=AXIS2_PLACEMENT_3D('',#10618,#8510,#8511);
#7594=AXIS2_PLACEMENT_3D('',#10619,#8512,#8513);
#7595=AXIS2_PLACEMENT_3D('',#10620,#8514,#8515);
#7596=AXIS2_PLACEMENT_3D('',#10621,#8516,#8517);
#7597=AXIS2_PLACEMENT_3D('',#10623,#8518,#8519);
#7598=AXIS2_PLACEMENT_3D('',#10626,#8521,#8522);
#7599=AXIS2_PLACEMENT_3D('',#10627,#8523,#8524);
#7600=AXIS2_PLACEMENT_3D('',#10636,#8529,#8530);
#7601=AXIS2_PLACEMENT_3D('',#10642,#8534,#8535);
#7602=AXIS2_PLACEMENT_3D('',#10648,#8539,#8540);
#7603=AXIS2_PLACEMENT_3D('',#10651,#8543,#8544);
#7604=AXIS2_PLACEMENT_3D('',#10652,#8545,#8546);
#7605=AXIS2_PLACEMENT_3D('',#10653,#8547,#8548);
#7606=AXIS2_PLACEMENT_3D('',#10654,#8549,#8550);
#7607=AXIS2_PLACEMENT_3D('',#10656,#8551,#8552);
#7608=AXIS2_PLACEMENT_3D('',#10659,#8554,#8555);
#7609=AXIS2_PLACEMENT_3D('',#10660,#8556,#8557);
#7610=AXIS2_PLACEMENT_3D('',#10662,#8558,#8559);
#7611=AXIS2_PLACEMENT_3D('',#10665,#8561,#8562);
#7612=AXIS2_PLACEMENT_3D('',#10666,#8563,#8564);
#7613=AXIS2_PLACEMENT_3D('',#10668,#8565,#8566);
#7614=AXIS2_PLACEMENT_3D('',#10671,#8568,#8569);
#7615=AXIS2_PLACEMENT_3D('',#10672,#8570,#8571);
#7616=AXIS2_PLACEMENT_3D('',#10674,#8572,#8573);
#7617=AXIS2_PLACEMENT_3D('',#10677,#8575,#8576);
#7618=AXIS2_PLACEMENT_3D('',#10678,#8577,#8578);
#7619=AXIS2_PLACEMENT_3D('',#10679,#8579,#8580);
#7620=AXIS2_PLACEMENT_3D('',#10681,#8581,#8582);
#7621=AXIS2_PLACEMENT_3D('',#10682,#8583,#8584);
#7622=AXIS2_PLACEMENT_3D('',#10685,#8586,#8587);
#7623=AXIS2_PLACEMENT_3D('',#10686,#8588,#8589);
#7624=AXIS2_PLACEMENT_3D('',#10687,#8590,#8591);
#7625=AXIS2_PLACEMENT_3D('',#10688,#8592,#8593);
#7626=AXIS2_PLACEMENT_3D('',#10689,#8594,#8595);
#7627=AXIS2_PLACEMENT_3D('',#10691,#8596,#8597);
#7628=AXIS2_PLACEMENT_3D('',#10694,#8599,#8600);
#7629=AXIS2_PLACEMENT_3D('',#10695,#8601,#8602);
#7630=AXIS2_PLACEMENT_3D('',#10697,#8603,#8604);
#7631=AXIS2_PLACEMENT_3D('',#10700,#8606,#8607);
#7632=AXIS2_PLACEMENT_3D('',#10701,#8608,#8609);
#7633=AXIS2_PLACEMENT_3D('',#10702,#8610,#8611);
#7634=AXIS2_PLACEMENT_3D('',#10703,#8612,#8613);
#7635=AXIS2_PLACEMENT_3D('',#10704,#8614,#8615);
#7636=AXIS2_PLACEMENT_3D('',#10706,#8616,#8617);
#7637=AXIS2_PLACEMENT_3D('',#10709,#8619,#8620);
#7638=AXIS2_PLACEMENT_3D('',#10710,#8621,#8622);
#7639=AXIS2_PLACEMENT_3D('',#10712,#8623,#8624);
#7640=AXIS2_PLACEMENT_3D('',#10715,#8626,#8627);
#7641=AXIS2_PLACEMENT_3D('',#10716,#8628,#8629);
#7642=AXIS2_PLACEMENT_3D('',#10718,#8630,#8631);
#7643=AXIS2_PLACEMENT_3D('',#10721,#8633,#8634);
#7644=AXIS2_PLACEMENT_3D('',#10722,#8635,#8636);
#7645=AXIS2_PLACEMENT_3D('',#10724,#8637,#8638);
#7646=AXIS2_PLACEMENT_3D('',#10725,#8639,#8640);
#7647=AXIS2_PLACEMENT_3D('',#10727,#8641,#8642);
#7648=AXIS2_PLACEMENT_3D('',#10730,#8644,#8645);
#7649=AXIS2_PLACEMENT_3D('',#10731,#8646,#8647);
#7650=AXIS2_PLACEMENT_3D('',#10733,#8648,#8649);
#7651=AXIS2_PLACEMENT_3D('',#10734,#8650,#8651);
#7652=AXIS2_PLACEMENT_3D('',#10736,#8653,#8654);
#7653=AXIS2_PLACEMENT_3D('',#10738,#8655,#8656);
#7654=AXIS2_PLACEMENT_3D('',#10741,#8658,#8659);
#7655=AXIS2_PLACEMENT_3D('',#10742,#8660,#8661);
#7656=AXIS2_PLACEMENT_3D('',#10743,#8662,#8663);
#7657=AXIS2_PLACEMENT_3D('',#10744,#8664,#8665);
#7658=AXIS2_PLACEMENT_3D('',#10745,#8666,#8667);
#7659=AXIS2_PLACEMENT_3D('',#10747,#8668,#8669);
#7660=AXIS2_PLACEMENT_3D('',#10749,#8670,#8671);
#7661=AXIS2_PLACEMENT_3D('',#10750,#8672,#8673);
#7662=AXIS2_PLACEMENT_3D('',#10752,#8674,#8675);
#7663=AXIS2_PLACEMENT_3D('',#10754,#8676,#8677);
#7664=AXIS2_PLACEMENT_3D('',#10755,#8678,#8679);
#7665=AXIS2_PLACEMENT_3D('',#10757,#8681,#8682);
#7666=AXIS2_PLACEMENT_3D('',#10760,#8684,#8685);
#7667=AXIS2_PLACEMENT_3D('',#10761,#8686,#8687);
#7668=AXIS2_PLACEMENT_3D('',#10763,#8688,#8689);
#7669=AXIS2_PLACEMENT_3D('',#10765,#8691,#8692);
#7670=AXIS2_PLACEMENT_3D('',#10766,#8693,#8694);
#7671=AXIS2_PLACEMENT_3D('',#10767,#8695,#8696);
#7672=AXIS2_PLACEMENT_3D('',#10768,#8697,#8698);
#7673=AXIS2_PLACEMENT_3D('',#10770,#8699,#8700);
#7674=AXIS2_PLACEMENT_3D('',#10773,#8702,#8703);
#7675=AXIS2_PLACEMENT_3D('',#10774,#8704,#8705);
#7676=AXIS2_PLACEMENT_3D('',#10776,#8706,#8707);
#7677=AXIS2_PLACEMENT_3D('',#10779,#8709,#8710);
#7678=AXIS2_PLACEMENT_3D('',#10780,#8711,#8712);
#7679=AXIS2_PLACEMENT_3D('',#10781,#8713,#8714);
#7680=AXIS2_PLACEMENT_3D('',#10782,#8715,#8716);
#7681=AXIS2_PLACEMENT_3D('',#10783,#8717,#8718);
#7682=AXIS2_PLACEMENT_3D('',#10785,#8719,#8720);
#7683=AXIS2_PLACEMENT_3D('',#10787,#8721,#8722);
#7684=AXIS2_PLACEMENT_3D('',#10788,#8723,#8724);
#7685=AXIS2_PLACEMENT_3D('',#10790,#8725,#8726);
#7686=AXIS2_PLACEMENT_3D('',#10792,#8727,#8728);
#7687=AXIS2_PLACEMENT_3D('',#10793,#8729,#8730);
#7688=AXIS2_PLACEMENT_3D('',#10795,#8732,#8733);
#7689=AXIS2_PLACEMENT_3D('',#10798,#8735,#8736);
#7690=AXIS2_PLACEMENT_3D('',#10799,#8737,#8738);
#7691=AXIS2_PLACEMENT_3D('',#10801,#8739,#8740);
#7692=AXIS2_PLACEMENT_3D('',#10803,#8742,#8743);
#7693=AXIS2_PLACEMENT_3D('',#10804,#8744,#8745);
#7694=AXIS2_PLACEMENT_3D('',#10805,#8746,#8747);
#7695=AXIS2_PLACEMENT_3D('',#10806,#8748,#8749);
#7696=AXIS2_PLACEMENT_3D('',#10808,#8750,#8751);
#7697=AXIS2_PLACEMENT_3D('',#10811,#8753,#8754);
#7698=AXIS2_PLACEMENT_3D('',#10812,#8755,#8756);
#7699=AXIS2_PLACEMENT_3D('',#10814,#8757,#8758);
#7700=AXIS2_PLACEMENT_3D('',#10817,#8760,#8761);
#7701=AXIS2_PLACEMENT_3D('',#10818,#8762,#8763);
#7702=AXIS2_PLACEMENT_3D('',#10819,#8764,#8765);
#7703=AXIS2_PLACEMENT_3D('',#10820,#8766,#8767);
#7704=AXIS2_PLACEMENT_3D('',#13222,#8768,#8769);
#7705=AXIS2_PLACEMENT_3D('',#13464,#8770,#8771);
#7706=AXIS2_PLACEMENT_3D('',#13465,#8772,#8773);
#7707=AXIS2_PLACEMENT_3D('',#13466,#8774,#8775);
#7708=AXIS2_PLACEMENT_3D('',#13467,#8776,#8777);
#7709=AXIS2_PLACEMENT_3D('',#13468,#8778,#8779);
#7710=AXIS2_PLACEMENT_3D('',#13471,#8780,#8781);
#7711=AXIS2_PLACEMENT_3D('',#13472,#8782,#8783);
#7712=AXIS2_PLACEMENT_3D('',#13473,#8784,#8785);
#7713=AXIS2_PLACEMENT_3D('',#13477,#8787,#8788);
#7714=AXIS2_PLACEMENT_3D('',#13479,#8789,#8790);
#7715=AXIS2_PLACEMENT_3D('',#13481,#8792,#8793);
#7716=AXIS2_PLACEMENT_3D('',#13492,#8798,#8799);
#7717=AXIS2_PLACEMENT_3D('',#13494,#8801,#8802);
#7718=AXIS2_PLACEMENT_3D('',#13495,#8803,#8804);
#7719=AXIS2_PLACEMENT_3D('',#13498,#8806,#8807);
#7720=AXIS2_PLACEMENT_3D('',#13499,#8808,#8809);
#7721=AXIS2_PLACEMENT_3D('',#13500,#8810,#8811);
#7722=AXIS2_PLACEMENT_3D('',#13502,#8812,#8813);
#7723=AXIS2_PLACEMENT_3D('',#13503,#8814,#8815);
#7724=AXIS2_PLACEMENT_3D('',#13504,#8816,#8817);
#7725=AXIS2_PLACEMENT_3D('',#13506,#8818,#8819);
#7726=AXIS2_PLACEMENT_3D('',#13508,#8821,#8822);
#7727=AXIS2_PLACEMENT_3D('',#13514,#8826,#8827);
#7728=AXIS2_PLACEMENT_3D('',#13517,#8830,#8831);
#7729=AXIS2_PLACEMENT_3D('',#13518,#8832,#8833);
#7730=AXIS2_PLACEMENT_3D('',#13519,#8834,#8835);
#7731=AXIS2_PLACEMENT_3D('',#13520,#8836,#8837);
#7732=AXIS2_PLACEMENT_3D('',#13523,#8838,#8839);
#7733=AXIS2_PLACEMENT_3D('',#13524,#8840,#8841);
#7734=AXIS2_PLACEMENT_3D('',#13525,#8842,#8843);
#7735=AXIS2_PLACEMENT_3D('',#13529,#8845,#8846);
#7736=AXIS2_PLACEMENT_3D('',#13531,#8847,#8848);
#7737=AXIS2_PLACEMENT_3D('',#13533,#8850,#8851);
#7738=AXIS2_PLACEMENT_3D('',#13544,#8856,#8857);
#7739=AXIS2_PLACEMENT_3D('',#13546,#8859,#8860);
#7740=AXIS2_PLACEMENT_3D('',#13547,#8861,#8862);
#7741=AXIS2_PLACEMENT_3D('',#13549,#8863,#8864);
#7742=AXIS2_PLACEMENT_3D('',#13551,#8866,#8867);
#7743=AXIS2_PLACEMENT_3D('',#13552,#8868,#8869);
#7744=AXIS2_PLACEMENT_3D('',#13554,#8870,#8871);
#7745=AXIS2_PLACEMENT_3D('',#13555,#8872,#8873);
#7746=AXIS2_PLACEMENT_3D('',#13556,#8874,#8875);
#7747=AXIS2_PLACEMENT_3D('',#13558,#8876,#8877);
#7748=AXIS2_PLACEMENT_3D('',#13560,#8879,#8880);
#7749=AXIS2_PLACEMENT_3D('',#13566,#8884,#8885);
#7750=AXIS2_PLACEMENT_3D('',#13569,#8888,#8889);
#7751=AXIS2_PLACEMENT_3D('',#13570,#8890,#8891);
#7752=AXIS2_PLACEMENT_3D('',#13571,#8892,#8893);
#7753=AXIS2_PLACEMENT_3D('',#13572,#8894,#8895);
#7754=AXIS2_PLACEMENT_3D('',#13581,#8900,#8901);
#7755=AXIS2_PLACEMENT_3D('',#13587,#8905,#8906);
#7756=AXIS2_PLACEMENT_3D('',#13593,#8910,#8911);
#7757=AXIS2_PLACEMENT_3D('',#13599,#8915,#8916);
#7758=AXIS2_PLACEMENT_3D('',#13605,#8920,#8921);
#7759=AXIS2_PLACEMENT_3D('',#13611,#8925,#8926);
#7760=AXIS2_PLACEMENT_3D('',#13617,#8930,#8931);
#7761=AXIS2_PLACEMENT_3D('',#13623,#8935,#8936);
#7762=AXIS2_PLACEMENT_3D('',#13629,#8940,#8941);
#7763=AXIS2_PLACEMENT_3D('',#13638,#8946,#8947);
#7764=AXIS2_PLACEMENT_3D('',#13644,#8951,#8952);
#7765=AXIS2_PLACEMENT_3D('',#13650,#8956,#8957);
#7766=AXIS2_PLACEMENT_3D('',#13656,#8961,#8962);
#7767=AXIS2_PLACEMENT_3D('',#13662,#8966,#8967);
#7768=AXIS2_PLACEMENT_3D('',#13668,#8971,#8972);
#7769=AXIS2_PLACEMENT_3D('',#13674,#8976,#8977);
#7770=AXIS2_PLACEMENT_3D('',#13680,#8981,#8982);
#7771=AXIS2_PLACEMENT_3D('',#13686,#8986,#8987);
#7772=AXIS2_PLACEMENT_3D('',#13695,#8992,#8993);
#7773=AXIS2_PLACEMENT_3D('',#13701,#8997,#8998);
#7774=AXIS2_PLACEMENT_3D('',#13707,#9002,#9003);
#7775=AXIS2_PLACEMENT_3D('',#13713,#9007,#9008);
#7776=AXIS2_PLACEMENT_3D('',#13719,#9012,#9013);
#7777=AXIS2_PLACEMENT_3D('',#13725,#9017,#9018);
#7778=AXIS2_PLACEMENT_3D('',#13731,#9022,#9023);
#7779=AXIS2_PLACEMENT_3D('',#13737,#9027,#9028);
#7780=AXIS2_PLACEMENT_3D('',#13743,#9032,#9033);
#7781=AXIS2_PLACEMENT_3D('',#13752,#9038,#9039);
#7782=AXIS2_PLACEMENT_3D('',#13758,#9043,#9044);
#7783=AXIS2_PLACEMENT_3D('',#13764,#9048,#9049);
#7784=AXIS2_PLACEMENT_3D('',#13770,#9053,#9054);
#7785=AXIS2_PLACEMENT_3D('',#13776,#9058,#9059);
#7786=AXIS2_PLACEMENT_3D('',#13782,#9063,#9064);
#7787=AXIS2_PLACEMENT_3D('',#13788,#9068,#9069);
#7788=AXIS2_PLACEMENT_3D('',#13794,#9073,#9074);
#7789=AXIS2_PLACEMENT_3D('',#13800,#9078,#9079);
#7790=AXIS2_PLACEMENT_3D('',#13802,#9080,#9081);
#7791=AXIS2_PLACEMENT_3D('',#13805,#9083,#9084);
#7792=AXIS2_PLACEMENT_3D('',#13806,#9085,#9086);
#7793=AXIS2_PLACEMENT_3D('',#13812,#9090,#9091);
#7794=AXIS2_PLACEMENT_3D('',#13818,#9095,#9096);
#7795=AXIS2_PLACEMENT_3D('',#13821,#9099,#9100);
#7796=AXIS2_PLACEMENT_3D('',#13827,#9104,#9105);
#7797=AXIS2_PLACEMENT_3D('',#13830,#9108,#9109);
#7798=AXIS2_PLACEMENT_3D('',#13836,#9113,#9114);
#7799=AXIS2_PLACEMENT_3D('',#13839,#9117,#9118);
#7800=AXIS2_PLACEMENT_3D('',#13842,#9121,#9122);
#7801=AXIS2_PLACEMENT_3D('',#13843,#9123,#9124);
#7802=AXIS2_PLACEMENT_3D('',#13844,#9125,#9126);
#7803=AXIS2_PLACEMENT_3D('',#13845,#9127,#9128);
#7804=AXIS2_PLACEMENT_3D('',#13847,#9129,#9130);
#7805=AXIS2_PLACEMENT_3D('',#13850,#9132,#9133);
#7806=AXIS2_PLACEMENT_3D('',#13851,#9134,#9135);
#7807=AXIS2_PLACEMENT_3D('',#13853,#9136,#9137);
#7808=AXIS2_PLACEMENT_3D('',#13854,#9138,#9139);
#7809=AXIS2_PLACEMENT_3D('',#13856,#9140,#9141);
#7810=AXIS2_PLACEMENT_3D('',#13859,#9143,#9144);
#7811=AXIS2_PLACEMENT_3D('',#13860,#9145,#9146);
#7812=AXIS2_PLACEMENT_3D('',#13862,#9147,#9148);
#7813=AXIS2_PLACEMENT_3D('',#13863,#9149,#9150);
#7814=AXIS2_PLACEMENT_3D('',#13865,#9151,#9152);
#7815=AXIS2_PLACEMENT_3D('',#13868,#9154,#9155);
#7816=AXIS2_PLACEMENT_3D('',#13869,#9156,#9157);
#7817=AXIS2_PLACEMENT_3D('',#13871,#9158,#9159);
#7818=AXIS2_PLACEMENT_3D('',#13872,#9160,#9161);
#7819=AXIS2_PLACEMENT_3D('',#13874,#9162,#9163);
#7820=AXIS2_PLACEMENT_3D('',#13877,#9165,#9166);
#7821=AXIS2_PLACEMENT_3D('',#13878,#9167,#9168);
#7822=AXIS2_PLACEMENT_3D('',#13880,#9169,#9170);
#7823=AXIS2_PLACEMENT_3D('',#13881,#9171,#9172);
#7824=AXIS2_PLACEMENT_3D('',#13883,#9173,#9174);
#7825=AXIS2_PLACEMENT_3D('',#13885,#9176,#9177);
#7826=AXIS2_PLACEMENT_3D('',#13887,#9178,#9179);
#7827=AXIS2_PLACEMENT_3D('',#13889,#9181,#9182);
#7828=AXIS2_PLACEMENT_3D('',#13891,#9183,#9184);
#7829=AXIS2_PLACEMENT_3D('',#13893,#9186,#9187);
#7830=AXIS2_PLACEMENT_3D('',#13895,#9188,#9189);
#7831=AXIS2_PLACEMENT_3D('',#13897,#9191,#9192);
#7832=AXIS2_PLACEMENT_3D('',#13906,#9197,#9198);
#7833=AXIS2_PLACEMENT_3D('',#13912,#9202,#9203);
#7834=AXIS2_PLACEMENT_3D('',#13918,#9207,#9208);
#7835=AXIS2_PLACEMENT_3D('',#13924,#9212,#9213);
#7836=AXIS2_PLACEMENT_3D('',#13930,#9217,#9218);
#7837=AXIS2_PLACEMENT_3D('',#13936,#9222,#9223);
#7838=AXIS2_PLACEMENT_3D('',#13942,#9227,#9228);
#7839=AXIS2_PLACEMENT_3D('',#13948,#9232,#9233);
#7840=AXIS2_PLACEMENT_3D('',#13954,#9237,#9238);
#7841=AXIS2_PLACEMENT_3D('',#13960,#9242,#9243);
#7842=AXIS2_PLACEMENT_3D('',#13966,#9247,#9248);
#7843=AXIS2_PLACEMENT_3D('',#13969,#9251,#9252);
#7844=AXIS2_PLACEMENT_3D('',#13970,#9253,#9254);
#7845=AXIS2_PLACEMENT_3D('',#13971,#9255,#9256);
#7846=AXIS2_PLACEMENT_3D('',#13972,#9257,#9258);
#7847=AXIS2_PLACEMENT_3D('',#13981,#9263,#9264);
#7848=AXIS2_PLACEMENT_3D('',#13987,#9268,#9269);
#7849=AXIS2_PLACEMENT_3D('',#13993,#9273,#9274);
#7850=AXIS2_PLACEMENT_3D('',#13999,#9278,#9279);
#7851=AXIS2_PLACEMENT_3D('',#14005,#9283,#9284);
#7852=AXIS2_PLACEMENT_3D('',#14008,#9287,#9288);
#7853=AXIS2_PLACEMENT_3D('',#14009,#9289,#9290);
#7854=AXIS2_PLACEMENT_3D('',#14010,#9291,#9292);
#7855=AXIS2_PLACEMENT_3D('',#14012,#9293,#9294);
#7856=AXIS2_PLACEMENT_3D('',#14014,#9295,#9296);
#7857=AXIS2_PLACEMENT_3D('',#14015,#9297,#9298);
#7858=AXIS2_PLACEMENT_3D('',#14018,#9300,#9301);
#7859=AXIS2_PLACEMENT_3D('',#14019,#9302,#9303);
#7860=AXIS2_PLACEMENT_3D('',#14020,#9304,#9305);
#7861=AXIS2_PLACEMENT_3D('',#14022,#9306,#9307);
#7862=AXIS2_PLACEMENT_3D('',#14023,#9308,#9309);
#7863=AXIS2_PLACEMENT_3D('',#14025,#9310,#9311);
#7864=AXIS2_PLACEMENT_3D('',#14027,#9313,#9314);
#7865=AXIS2_PLACEMENT_3D('',#14029,#9315,#9316);
#7866=AXIS2_PLACEMENT_3D('',#14031,#9318,#9319);
#7867=AXIS2_PLACEMENT_3D('',#14033,#9320,#9321);
#7868=AXIS2_PLACEMENT_3D('',#14035,#9323,#9324);
#7869=AXIS2_PLACEMENT_3D('',#14037,#9325,#9326);
#7870=AXIS2_PLACEMENT_3D('',#14038,#9327,#9328);
#7871=AXIS2_PLACEMENT_3D('',#14040,#9329,#9330);
#7872=AXIS2_PLACEMENT_3D('',#14042,#9332,#9333);
#7873=AXIS2_PLACEMENT_3D('',#14044,#9335,#9336);
#7874=AXIS2_PLACEMENT_3D('',#14045,#9337,#9338);
#7875=AXIS2_PLACEMENT_3D('',#14047,#9339,#9340);
#7876=AXIS2_PLACEMENT_3D('',#14048,#9341,#9342);
#7877=AXIS2_PLACEMENT_3D('',#14050,#9343,#9344);
#7878=AXIS2_PLACEMENT_3D('',#14052,#9346,#9347);
#7879=AXIS2_PLACEMENT_3D('',#14054,#9348,#9349);
#7880=AXIS2_PLACEMENT_3D('',#14056,#9351,#9352);
#7881=AXIS2_PLACEMENT_3D('',#14058,#9353,#9354);
#7882=AXIS2_PLACEMENT_3D('',#14060,#9356,#9357);
#7883=AXIS2_PLACEMENT_3D('',#14062,#9358,#9359);
#7884=AXIS2_PLACEMENT_3D('',#14063,#9360,#9361);
#7885=AXIS2_PLACEMENT_3D('',#14065,#9362,#9363);
#7886=AXIS2_PLACEMENT_3D('',#14067,#9365,#9366);
#7887=AXIS2_PLACEMENT_3D('',#14069,#9367,#9368);
#7888=AXIS2_PLACEMENT_3D('',#14071,#9370,#9371);
#7889=AXIS2_PLACEMENT_3D('',#14073,#9372,#9373);
#7890=AXIS2_PLACEMENT_3D('',#14075,#9375,#9376);
#7891=AXIS2_PLACEMENT_3D('',#14076,#9377,#9378);
#7892=AXIS2_PLACEMENT_3D('',#14085,#9383,#9384);
#7893=AXIS2_PLACEMENT_3D('',#14091,#9388,#9389);
#7894=AXIS2_PLACEMENT_3D('',#14097,#9393,#9394);
#7895=AXIS2_PLACEMENT_3D('',#14103,#9398,#9399);
#7896=AXIS2_PLACEMENT_3D('',#14109,#9403,#9404);
#7897=AXIS2_PLACEMENT_3D('',#14112,#9407,#9408);
#7898=AXIS2_PLACEMENT_3D('',#14113,#9409,#9410);
#7899=AXIS2_PLACEMENT_3D('',#14114,#9411,#9412);
#7900=AXIS2_PLACEMENT_3D('',#14115,#9413,#9414);
#7901=AXIS2_PLACEMENT_3D('',#14124,#9419,#9420);
#7902=AXIS2_PLACEMENT_3D('',#14130,#9424,#9425);
#7903=AXIS2_PLACEMENT_3D('',#14137,#9429,#9430);
#7904=AXIS2_PLACEMENT_3D('',#14138,#9431,#9432);
#7905=AXIS2_PLACEMENT_3D('',#14152,#9440,#9441);
#7906=AXIS2_PLACEMENT_3D('',#14156,#9444,#9445);
#7907=AXIS2_PLACEMENT_3D('',#14160,#9448,#9449);
#7908=AXIS2_PLACEMENT_3D('',#14170,#9455,#9456);
#7909=AXIS2_PLACEMENT_3D('',#14172,#9458,#9459);
#7910=AXIS2_PLACEMENT_3D('',#14176,#9461,#9462);
#7911=AXIS2_PLACEMENT_3D('',#14178,#9464,#9465);
#7912=AXIS2_PLACEMENT_3D('',#14180,#9466,#9467);
#7913=AXIS2_PLACEMENT_3D('',#14183,#9469,#9470);
#7914=AXIS2_PLACEMENT_3D('',#14185,#9471,#9472);
#7915=AXIS2_PLACEMENT_3D('',#14186,#9473,#9474);
#7916=AXIS2_PLACEMENT_3D('',#14187,#9475,#9476);
#7917=AXIS2_PLACEMENT_3D('',#14189,#9478,#9479);
#7918=AXIS2_PLACEMENT_3D('',#14191,#9481,#9482);
#7919=AXIS2_PLACEMENT_3D('',#14193,#9484,#9485);
#7920=AXIS2_PLACEMENT_3D('',#14194,#9486,#9487);
#7921=AXIS2_PLACEMENT_3D('',#14195,#9488,#9489);
#7922=AXIS2_PLACEMENT_3D('',#14197,#9490,#9491);
#7923=AXIS2_PLACEMENT_3D('',#14200,#9493,#9494);
#7924=AXIS2_PLACEMENT_3D('',#14201,#9495,#9496);
#7925=AXIS2_PLACEMENT_3D('',#14204,#9498,#9499);
#7926=AXIS2_PLACEMENT_3D('',#14205,#9500,#9501);
#7927=AXIS2_PLACEMENT_3D('',#14207,#9502,#9503);
#7928=AXIS2_PLACEMENT_3D('',#14208,#9504,#9505);
#7929=AXIS2_PLACEMENT_3D('',#14211,#9507,#9508);
#7930=AXIS2_PLACEMENT_3D('',#14212,#9509,#9510);
#7931=AXIS2_PLACEMENT_3D('',#14213,#9511,#9512);
#7932=AXIS2_PLACEMENT_3D('',#14214,#9513,#9514);
#7933=AXIS2_PLACEMENT_3D('',#14215,#9515,#9516);
#7934=AXIS2_PLACEMENT_3D('',#14217,#9517,#9518);
#7935=AXIS2_PLACEMENT_3D('',#14220,#9520,#9521);
#7936=AXIS2_PLACEMENT_3D('',#14221,#9522,#9523);
#7937=AXIS2_PLACEMENT_3D('',#14230,#9528,#9529);
#7938=AXIS2_PLACEMENT_3D('',#14236,#9533,#9534);
#7939=AXIS2_PLACEMENT_3D('',#14242,#9538,#9539);
#7940=AXIS2_PLACEMENT_3D('',#14248,#9543,#9544);
#7941=AXIS2_PLACEMENT_3D('',#14258,#9550,#9551);
#7942=AXIS2_PLACEMENT_3D('',#14260,#9552,#9553);
#7943=AXIS2_PLACEMENT_3D('',#14263,#9555,#9556);
#7944=AXIS2_PLACEMENT_3D('',#14264,#9557,#9558);
#7945=AXIS2_PLACEMENT_3D('',#14266,#9559,#9560);
#7946=AXIS2_PLACEMENT_3D('',#14269,#9562,#9563);
#7947=AXIS2_PLACEMENT_3D('',#14270,#9564,#9565);
#7948=AXIS2_PLACEMENT_3D('',#14272,#9566,#9567);
#7949=AXIS2_PLACEMENT_3D('',#14275,#9569,#9570);
#7950=AXIS2_PLACEMENT_3D('',#14276,#9571,#9572);
#7951=AXIS2_PLACEMENT_3D('',#14281,#9574,#9575);
#7952=AXIS2_PLACEMENT_3D('',#14284,#9577,#9578);
#7953=AXIS2_PLACEMENT_3D('',#14285,#9579,#9580);
#7954=AXIS2_PLACEMENT_3D('',#14287,#9582,#9583);
#7955=AXIS2_PLACEMENT_3D('',#14295,#9587,#9588);
#7956=AXIS2_PLACEMENT_3D('',#14299,#9591,#9592);
#7957=AXIS2_PLACEMENT_3D('',#14301,#9593,#9594);
#7958=AXIS2_PLACEMENT_3D('',#14303,#9595,#9596);
#7959=AXIS2_PLACEMENT_3D('',#14305,#9597,#9598);
#7960=AXIS2_PLACEMENT_3D('',#14306,#9599,#9600);
#7961=AXIS2_PLACEMENT_3D('',#14309,#9602,#9603);
#7962=AXIS2_PLACEMENT_3D('',#14310,#9604,#9605);
#7963=AXIS2_PLACEMENT_3D('',#14325,#9614,#9615);
#7964=AXIS2_PLACEMENT_3D('',#14328,#9617,#9618);
#7965=AXIS2_PLACEMENT_3D('',#14329,#9619,#9620);
#7966=AXIS2_PLACEMENT_3D('',#14330,#9621,#9622);
#7967=AXIS2_PLACEMENT_3D('',#14331,#9623,#9624);
#7968=AXIS2_PLACEMENT_3D('',#14332,#9625,#9626);
#7969=AXIS2_PLACEMENT_3D('',#14335,#9628,#9629);
#7970=AXIS2_PLACEMENT_3D('',#14336,#9630,#9631);
#7971=AXIS2_PLACEMENT_3D('',#14339,#9633,#9634);
#7972=AXIS2_PLACEMENT_3D('',#14340,#9635,#9636);
#7973=AXIS2_PLACEMENT_3D('',#14346,#9640,#9641);
#7974=AXIS2_PLACEMENT_3D('',#14350,#9644,#9645);
#7975=AXIS2_PLACEMENT_3D('',#14354,#9648,#9649);
#7976=AXIS2_PLACEMENT_3D('',#14358,#9652,#9653);
#7977=AXIS2_PLACEMENT_3D('',#14360,#9655,#9656);
#7978=AXIS2_PLACEMENT_3D('',#14362,#9658,#9659);
#7979=AXIS2_PLACEMENT_3D('',#14366,#9662,#9663);
#7980=AXIS2_PLACEMENT_3D('',#14372,#9667,#9668);
#7981=AXIS2_PLACEMENT_3D('',#14375,#9671,#9672);
#7982=AXIS2_PLACEMENT_3D('',#14376,#9673,#9674);
#7983=AXIS2_PLACEMENT_3D('',#14377,#9675,#9676);
#7984=AXIS2_PLACEMENT_3D('',#14378,#9677,#9678);
#7985=AXIS2_PLACEMENT_3D('',#14380,#9679,#9680);
#7986=AXIS2_PLACEMENT_3D('',#14383,#9682,#9683);
#7987=AXIS2_PLACEMENT_3D('',#14384,#9684,#9685);
#7988=AXIS2_PLACEMENT_3D('',#14386,#9686,#9687);
#7989=AXIS2_PLACEMENT_3D('',#14389,#9689,#9690);
#7990=AXIS2_PLACEMENT_3D('',#14390,#9691,#9692);
#7991=AXIS2_PLACEMENT_3D('',#14391,#9693,#9694);
#7992=AXIS2_PLACEMENT_3D('',#14392,#9695,#9696);
#7993=AXIS2_PLACEMENT_3D('',#14393,#9697,#9698);
#7994=AXIS2_PLACEMENT_3D('',#14395,#9699,#9700);
#7995=AXIS2_PLACEMENT_3D('',#14398,#9702,#9703);
#7996=AXIS2_PLACEMENT_3D('',#14399,#9704,#9705);
#7997=AXIS2_PLACEMENT_3D('',#14400,#9706,#9707);
#7998=AXIS2_PLACEMENT_3D('',#14402,#9708,#9709);
#7999=AXIS2_PLACEMENT_3D('',#14405,#9711,#9712);
#8000=AXIS2_PLACEMENT_3D('',#14406,#9713,#9714);
#8001=AXIS2_PLACEMENT_3D('',#14407,#9715,#9716);
#8002=AXIS2_PLACEMENT_3D('',#14409,#9717,#9718);
#8003=AXIS2_PLACEMENT_3D('',#14411,#9719,#9720);
#8004=AXIS2_PLACEMENT_3D('',#14412,#9721,#9722);
#8005=AXIS2_PLACEMENT_3D('',#14414,#9723,#9724);
#8006=AXIS2_PLACEMENT_3D('',#14416,#9726,#9727);
#8007=AXIS2_PLACEMENT_3D('',#14417,#9728,#9729);
#8008=AXIS2_PLACEMENT_3D('',#14420,#9731,#9732);
#8009=AXIS2_PLACEMENT_3D('',#14421,#9733,#9734);
#8010=AXIS2_PLACEMENT_3D('',#14422,#9735,#9736);
#8011=AXIS2_PLACEMENT_3D('',#14423,#9737,#9738);
#8012=AXIS2_PLACEMENT_3D('',#14425,#9739,#9740);
#8013=AXIS2_PLACEMENT_3D('',#14428,#9742,#9743);
#8014=AXIS2_PLACEMENT_3D('',#14429,#9744,#9745);
#8015=AXIS2_PLACEMENT_3D('',#14431,#9746,#9747);
#8016=AXIS2_PLACEMENT_3D('',#14434,#9749,#9750);
#8017=AXIS2_PLACEMENT_3D('',#14435,#9751,#9752);
#8018=AXIS2_PLACEMENT_3D('',#14436,#9753,#9754);
#8019=AXIS2_PLACEMENT_3D('',#14437,#9755,#9756);
#8020=AXIS2_PLACEMENT_3D('',#14438,#9757,#9758);
#8021=AXIS2_PLACEMENT_3D('',#14440,#9759,#9760);
#8022=AXIS2_PLACEMENT_3D('',#14443,#9762,#9763);
#8023=AXIS2_PLACEMENT_3D('',#14444,#9764,#9765);
#8024=AXIS2_PLACEMENT_3D('',#14446,#9766,#9767);
#8025=AXIS2_PLACEMENT_3D('',#14449,#9769,#9770);
#8026=AXIS2_PLACEMENT_3D('',#14450,#9771,#9772);
#8027=AXIS2_PLACEMENT_3D('',#14451,#9773,#9774);
#8028=AXIS2_PLACEMENT_3D('',#14460,#9779,#9780);
#8029=AXIS2_PLACEMENT_3D('',#14466,#9784,#9785);
#8030=AXIS2_PLACEMENT_3D('',#14472,#9789,#9790);
#8031=AXIS2_PLACEMENT_3D('',#14475,#9793,#9794);
#8032=AXIS2_PLACEMENT_3D('',#14476,#9795,#9796);
#8033=AXIS2_PLACEMENT_3D('',#14477,#9797,#9798);
#8034=AXIS2_PLACEMENT_3D('',#14478,#9799,#9800);
#8035=AXIS2_PLACEMENT_3D('',#14487,#9805,#9806);
#8036=AXIS2_PLACEMENT_3D('',#14493,#9810,#9811);
#8037=AXIS2_PLACEMENT_3D('',#14499,#9815,#9816);
#8038=AXIS2_PLACEMENT_3D('',#14502,#9819,#9820);
#8039=AXIS2_PLACEMENT_3D('',#14503,#9821,#9822);
#8040=AXIS2_PLACEMENT_3D('',#14504,#9823,#9824);
#8041=AXIS2_PLACEMENT_3D('',#14505,#9825,#9826);
#8042=AXIS2_PLACEMENT_3D('',#14507,#9827,#9828);
#8043=AXIS2_PLACEMENT_3D('',#14510,#9830,#9831);
#8044=AXIS2_PLACEMENT_3D('',#14511,#9832,#9833);
#8045=AXIS2_PLACEMENT_3D('',#14512,#9834,#9835);
#8046=AXIS2_PLACEMENT_3D('',#14514,#9836,#9837);
#8047=AXIS2_PLACEMENT_3D('',#14515,#9838,#9839);
#8048=AXIS2_PLACEMENT_3D('',#14518,#9841,#9842);
#8049=AXIS2_PLACEMENT_3D('',#14519,#9843,#9844);
#8050=AXIS2_PLACEMENT_3D('',#14520,#9845,#9846);
#8051=AXIS2_PLACEMENT_3D('',#14521,#9847,#9848);
#8052=AXIS2_PLACEMENT_3D('',#14522,#9849,#9850);
#8053=AXIS2_PLACEMENT_3D('',#14526,#9852,#9853);
#8054=AXIS2_PLACEMENT_3D('',#14527,#9854,#9855);
#8055=AXIS2_PLACEMENT_3D('',#14531,#9857,#9858);
#8056=AXIS2_PLACEMENT_3D('',#14534,#9860,#9861);
#8057=AXIS2_PLACEMENT_3D('',#14536,#9862,#9863);
#8058=AXIS2_PLACEMENT_3D('',#14538,#9865,#9866);
#8059=AXIS2_PLACEMENT_3D('',#14542,#9868,#9869);
#8060=AXIS2_PLACEMENT_3D('',#14543,#9870,#9871);
#8061=AXIS2_PLACEMENT_3D('',#14547,#9873,#9874);
#8062=AXIS2_PLACEMENT_3D('',#14550,#9876,#9877);
#8063=AXIS2_PLACEMENT_3D('',#14552,#9878,#9879);
#8064=AXIS2_PLACEMENT_3D('',#14554,#9881,#9882);
#8065=AXIS2_PLACEMENT_3D('',#14558,#9884,#9885);
#8066=AXIS2_PLACEMENT_3D('',#14559,#9886,#9887);
#8067=AXIS2_PLACEMENT_3D('',#14563,#9889,#9890);
#8068=AXIS2_PLACEMENT_3D('',#14566,#9892,#9893);
#8069=AXIS2_PLACEMENT_3D('',#14568,#9894,#9895);
#8070=AXIS2_PLACEMENT_3D('',#14570,#9897,#9898);
#8071=AXIS2_PLACEMENT_3D('',#14574,#9900,#9901);
#8072=AXIS2_PLACEMENT_3D('',#14575,#9902,#9903);
#8073=AXIS2_PLACEMENT_3D('',#14579,#9905,#9906);
#8074=AXIS2_PLACEMENT_3D('',#14582,#9908,#9909);
#8075=AXIS2_PLACEMENT_3D('',#14584,#9910,#9911);
#8076=AXIS2_PLACEMENT_3D('',#14586,#9913,#9914);
#8077=AXIS2_PLACEMENT_3D('',#14597,#9921,#9922);
#8078=AXIS2_PLACEMENT_3D('',#14608,#9929,#9930);
#8079=AXIS2_PLACEMENT_3D('',#14627,#9941,#9942);
#8080=AXIS2_PLACEMENT_3D('',#14631,#9945,#9946);
#8081=AXIS2_PLACEMENT_3D('',#14635,#9949,#9950);
#8082=AXIS2_PLACEMENT_3D('',#14639,#9953,#9954);
#8083=AXIS2_PLACEMENT_3D('',#14643,#9957,#9958);
#8084=AXIS2_PLACEMENT_3D('',#14645,#9960,#9961);
#8085=AXIS2_PLACEMENT_3D('',#14649,#9964,#9965);
#8086=AXIS2_PLACEMENT_3D('',#14653,#9968,#9969);
#8087=AXIS2_PLACEMENT_3D('',#14657,#9972,#9973);
#8088=AXIS2_PLACEMENT_3D('',#14661,#9976,#9977);
#8089=AXIS2_PLACEMENT_3D('',#14663,#9979,#9980);
#8090=AXIS2_PLACEMENT_3D('',#14664,#9981,#9982);
#8091=AXIS2_PLACEMENT_3D('',#14665,#9983,#9984);
#8092=AXIS2_PLACEMENT_3D('',#14674,#9989,#9990);
#8093=AXIS2_PLACEMENT_3D('',#14680,#9994,#9995);
#8094=AXIS2_PLACEMENT_3D('',#14686,#9999,#10000);
#8095=AXIS2_PLACEMENT_3D('',#14692,#10004,#10005);
#8096=AXIS2_PLACEMENT_3D('',#14698,#10009,#10010);
#8097=AXIS2_PLACEMENT_3D('',#14704,#10014,#10015);
#8098=AXIS2_PLACEMENT_3D('',#14710,#10019,#10020);
#8099=AXIS2_PLACEMENT_3D('',#14713,#10023,#10024);
#8100=AXIS2_PLACEMENT_3D('',#14714,#10025,#10026);
#8101=AXIS2_PLACEMENT_3D('',#14715,#10027,#10028);
#8102=AXIS2_PLACEMENT_3D('',#14716,#10029,#10030);
#8103=AXIS2_PLACEMENT_3D('',#14725,#10035,#10036);
#8104=AXIS2_PLACEMENT_3D('',#14731,#10040,#10041);
#8105=AXIS2_PLACEMENT_3D('',#14737,#10045,#10046);
#8106=AXIS2_PLACEMENT_3D('',#14743,#10050,#10051);
#8107=AXIS2_PLACEMENT_3D('',#14749,#10055,#10056);
#8108=AXIS2_PLACEMENT_3D('',#14755,#10060,#10061);
#8109=AXIS2_PLACEMENT_3D('',#14761,#10065,#10066);
#8110=AXIS2_PLACEMENT_3D('',#14764,#10069,#10070);
#8111=AXIS2_PLACEMENT_3D('',#14765,#10071,#10072);
#8112=AXIS2_PLACEMENT_3D('',#14766,#10073,#10074);
#8113=AXIS2_PLACEMENT_3D('',#14767,#10075,#10076);
#8114=AXIS2_PLACEMENT_3D('',#14768,#10077,#10078);
#8115=AXIS2_PLACEMENT_3D('',#14769,#10079,#10080);
#8116=AXIS2_PLACEMENT_3D('',#14770,#10081,#10082);
#8117=AXIS2_PLACEMENT_3D('',#14779,#10087,#10088);
#8118=AXIS2_PLACEMENT_3D('',#14785,#10092,#10093);
#8119=AXIS2_PLACEMENT_3D('',#14791,#10097,#10098);
#8120=AXIS2_PLACEMENT_3D('',#14797,#10102,#10103);
#8121=AXIS2_PLACEMENT_3D('',#14803,#10107,#10108);
#8122=AXIS2_PLACEMENT_3D('',#14806,#10111,#10112);
#8123=AXIS2_PLACEMENT_3D('',#14807,#10113,#10114);
#8124=AXIS2_PLACEMENT_3D('',#14808,#10115,#10116);
#8125=AXIS2_PLACEMENT_3D('',#14810,#10117,#10118);
#8126=AXIS2_PLACEMENT_3D('',#14811,#10119,#10120);
#8127=AXIS2_PLACEMENT_3D('',#14813,#10121,#10122);
#8128=AXIS2_PLACEMENT_3D('',#14814,#10123,#10124);
#8129=AXIS2_PLACEMENT_3D('',#14816,#10125,#10126);
#8130=AXIS2_PLACEMENT_3D('',#14818,#10128,#10129);
#8131=AXIS2_PLACEMENT_3D('',#14820,#10130,#10131);
#8132=AXIS2_PLACEMENT_3D('',#14822,#10133,#10134);
#8133=AXIS2_PLACEMENT_3D('',#14824,#10135,#10136);
#8134=AXIS2_PLACEMENT_3D('',#14826,#10138,#10139);
#8135=AXIS2_PLACEMENT_3D('',#14828,#10140,#10141);
#8136=AXIS2_PLACEMENT_3D('',#14829,#10142,#10143);
#8137=AXIS2_PLACEMENT_3D('',#14831,#10144,#10145);
#8138=AXIS2_PLACEMENT_3D('',#14833,#10147,#10148);
#8139=AXIS2_PLACEMENT_3D('',#14835,#10150,#10151);
#8140=AXIS2_PLACEMENT_3D('',#14836,#10152,#10153);
#8141=AXIS2_PLACEMENT_3D('',#14838,#10154,#10155);
#8142=AXIS2_PLACEMENT_3D('',#14839,#10156,#10157);
#8143=AXIS2_PLACEMENT_3D('',#14841,#10158,#10159);
#8144=AXIS2_PLACEMENT_3D('',#14843,#10161,#10162);
#8145=AXIS2_PLACEMENT_3D('',#14845,#10163,#10164);
#8146=AXIS2_PLACEMENT_3D('',#14847,#10166,#10167);
#8147=AXIS2_PLACEMENT_3D('',#14849,#10168,#10169);
#8148=AXIS2_PLACEMENT_3D('',#14851,#10171,#10172);
#8149=AXIS2_PLACEMENT_3D('',#14853,#10173,#10174);
#8150=AXIS2_PLACEMENT_3D('',#14854,#10175,#10176);
#8151=AXIS2_PLACEMENT_3D('',#14856,#10177,#10178);
#8152=AXIS2_PLACEMENT_3D('',#14858,#10180,#10181);
#8153=AXIS2_PLACEMENT_3D('',#14860,#10182,#10183);
#8154=AXIS2_PLACEMENT_3D('',#14862,#10185,#10186);
#8155=AXIS2_PLACEMENT_3D('',#14864,#10187,#10188);
#8156=AXIS2_PLACEMENT_3D('',#14866,#10190,#10191);
#8157=AXIS2_PLACEMENT_3D('',#14867,#10192,#10193);
#8158=AXIS2_PLACEMENT_3D('',#14876,#10198,#10199);
#8159=AXIS2_PLACEMENT_3D('',#14882,#10203,#10204);
#8160=AXIS2_PLACEMENT_3D('',#14888,#10208,#10209);
#8161=AXIS2_PLACEMENT_3D('',#14894,#10213,#10214);
#8162=AXIS2_PLACEMENT_3D('',#14900,#10218,#10219);
#8163=AXIS2_PLACEMENT_3D('',#14903,#10222,#10223);
#8164=AXIS2_PLACEMENT_3D('',#14904,#10224,#10225);
#8165=AXIS2_PLACEMENT_3D('',#14905,#10226,#10227);
#8166=AXIS2_PLACEMENT_3D('',#14906,#10228,#10229);
#8167=AXIS2_PLACEMENT_3D('',#14907,#10230,#10231);
#8168=AXIS2_PLACEMENT_3D('',#14908,#10232,#10233);
#8169=AXIS2_PLACEMENT_3D('',#14909,#10234,#10235);
#8170=AXIS2_PLACEMENT_3D('',#14910,#10236,#10237);
#8171=AXIS2_PLACEMENT_3D('',#14911,#10238,#10239);
#8172=AXIS2_PLACEMENT_3D('',#14912,#10240,#10241);
#8173=AXIS2_PLACEMENT_3D('',#14913,#10242,#10243);
#8174=AXIS2_PLACEMENT_3D('',#14914,#10244,#10245);
#8175=AXIS2_PLACEMENT_3D('',#14915,#10246,#10247);
#8176=AXIS2_PLACEMENT_3D('',#14916,#10248,#10249);
#8177=AXIS2_PLACEMENT_3D('',#14917,#10250,#10251);
#8178=AXIS2_PLACEMENT_3D('',#14918,#10252,#10253);
#8179=AXIS2_PLACEMENT_3D('',#14919,#10254,#10255);
#8180=AXIS2_PLACEMENT_3D('',#14920,#10256,#10257);
#8181=AXIS2_PLACEMENT_3D('',#14921,#10258,#10259);
#8182=AXIS2_PLACEMENT_3D('',#14922,#10260,#10261);
#8183=AXIS2_PLACEMENT_3D('',#14923,#10262,#10263);
#8184=AXIS2_PLACEMENT_3D('',#14924,#10264,#10265);
#8185=AXIS2_PLACEMENT_3D('',#14925,#10266,#10267);
#8186=AXIS2_PLACEMENT_3D('',#14926,#10268,#10269);
#8187=AXIS2_PLACEMENT_3D('',#14927,#10270,#10271);
#8188=AXIS2_PLACEMENT_3D('',#14928,#10272,#10273);
#8189=AXIS2_PLACEMENT_3D('',#14929,#10274,#10275);
#8190=AXIS2_PLACEMENT_3D('',#14930,#10276,#10277);
#8191=AXIS2_PLACEMENT_3D('',#14931,#10278,#10279);
#8192=AXIS2_PLACEMENT_3D('',#14932,#10280,#10281);
#8193=AXIS2_PLACEMENT_3D('',#14933,#10282,#10283);
#8194=AXIS2_PLACEMENT_3D('',#14934,#10284,#10285);
#8195=AXIS2_PLACEMENT_3D('',#14935,#10286,#10287);
#8196=AXIS2_PLACEMENT_3D('',#14936,#10288,#10289);
#8197=AXIS2_PLACEMENT_3D('',#14937,#10290,#10291);
#8198=AXIS2_PLACEMENT_3D('',#14938,#10292,#10293);
#8199=AXIS2_PLACEMENT_3D('',#14939,#10294,#10295);
#8200=AXIS2_PLACEMENT_3D('',#14940,#10296,#10297);
#8201=AXIS2_PLACEMENT_3D('',#14941,#10298,#10299);
#8202=AXIS2_PLACEMENT_3D('',#14942,#10300,#10301);
#8203=AXIS2_PLACEMENT_3D('',#14943,#10302,#10303);
#8204=AXIS2_PLACEMENT_3D('',#14944,#10304,#10305);
#8205=AXIS2_PLACEMENT_3D('',#14945,#10306,#10307);
#8206=AXIS2_PLACEMENT_3D('',#14946,#10308,#10309);
#8207=AXIS2_PLACEMENT_3D('',#14947,#10310,#10311);
#8208=AXIS2_PLACEMENT_3D('',#14948,#10312,#10313);
#8209=AXIS2_PLACEMENT_3D('',#14949,#10314,#10315);
#8210=AXIS2_PLACEMENT_3D('',#14950,#10316,#10317);
#8211=AXIS2_PLACEMENT_3D('',#14951,#10318,#10319);
#8212=AXIS2_PLACEMENT_3D('',#14952,#10320,#10321);
#8213=AXIS2_PLACEMENT_3D('',#14953,#10322,#10323);
#8214=AXIS2_PLACEMENT_3D('',#14954,#10324,#10325);
#8215=AXIS2_PLACEMENT_3D('',#14955,#10326,#10327);
#8216=AXIS2_PLACEMENT_3D('',#14956,#10328,#10329);
#8217=AXIS2_PLACEMENT_3D('',#14957,#10330,#10331);
#8218=AXIS2_PLACEMENT_3D('',#14958,#10332,#10333);
#8219=AXIS2_PLACEMENT_3D('',#14959,#10334,#10335);
#8220=AXIS2_PLACEMENT_3D('',#14960,#10336,#10337);
#8221=DIRECTION('axis',(0.,0.,1.));
#8222=DIRECTION('refdir',(1.,0.,0.));
#8223=DIRECTION('axis',(0.,0.,1.));
#8224=DIRECTION('refdir',(1.,0.,0.));
#8225=DIRECTION('axis',(0.,0.,1.));
#8226=DIRECTION('refdir',(1.,0.,0.));
#8227=DIRECTION('center_axis',(0.,0.,1.));
#8228=DIRECTION('ref_axis',(1.,0.,0.));
#8229=DIRECTION('center_axis',(0.,0.,1.));
#8230=DIRECTION('ref_axis',(1.,0.,0.));
#8231=DIRECTION('',(0.,0.,1.));
#8232=DIRECTION('center_axis',(0.,0.,-1.));
#8233=DIRECTION('ref_axis',(1.,0.,0.));
#8234=DIRECTION('center_axis',(0.,0.,1.));
#8235=DIRECTION('ref_axis',(1.,0.,0.));
#8236=DIRECTION('center_axis',(0.,0.,1.));
#8237=DIRECTION('ref_axis',(1.,0.,0.));
#8238=DIRECTION('center_axis',(0.,0.,1.));
#8239=DIRECTION('ref_axis',(1.,0.,0.));
#8240=DIRECTION('',(0.,0.,1.));
#8241=DIRECTION('center_axis',(0.,0.,-1.));
#8242=DIRECTION('ref_axis',(1.,0.,0.));
#8243=DIRECTION('center_axis',(0.,0.,1.));
#8244=DIRECTION('ref_axis',(1.,0.,0.));
#8245=DIRECTION('center_axis',(0.,0.,1.));
#8246=DIRECTION('ref_axis',(1.,0.,0.));
#8247=DIRECTION('center_axis',(0.,0.,1.));
#8248=DIRECTION('ref_axis',(1.,0.,0.));
#8249=DIRECTION('',(0.,0.,1.));
#8250=DIRECTION('center_axis',(0.,0.,-1.));
#8251=DIRECTION('ref_axis',(1.,0.,0.));
#8252=DIRECTION('center_axis',(0.,0.,1.));
#8253=DIRECTION('ref_axis',(1.,0.,0.));
#8254=DIRECTION('center_axis',(0.,0.,1.));
#8255=DIRECTION('ref_axis',(1.,0.,0.));
#8256=DIRECTION('center_axis',(0.,0.,1.));
#8257=DIRECTION('ref_axis',(1.,0.,0.));
#8258=DIRECTION('',(0.,0.,1.));
#8259=DIRECTION('center_axis',(0.,0.,-1.));
#8260=DIRECTION('ref_axis',(1.,0.,0.));
#8261=DIRECTION('center_axis',(0.,0.,1.));
#8262=DIRECTION('ref_axis',(1.,0.,0.));
#8263=DIRECTION('center_axis',(0.,0.,1.));
#8264=DIRECTION('ref_axis',(1.,0.,0.));
#8265=DIRECTION('center_axis',(0.,0.,1.));
#8266=DIRECTION('ref_axis',(1.,0.,0.));
#8267=DIRECTION('',(0.,0.,1.));
#8268=DIRECTION('center_axis',(0.,0.,-1.));
#8269=DIRECTION('ref_axis',(1.,0.,0.));
#8270=DIRECTION('center_axis',(0.,1.,0.));
#8271=DIRECTION('ref_axis',(-1.,0.,0.));
#8272=DIRECTION('',(-1.,0.,0.));
#8273=DIRECTION('',(0.,0.,1.));
#8274=DIRECTION('',(-1.,0.,0.));
#8275=DIRECTION('',(0.,0.,1.));
#8276=DIRECTION('center_axis',(1.,0.,0.));
#8277=DIRECTION('ref_axis',(0.,1.,0.));
#8278=DIRECTION('',(0.,1.,0.));
#8279=DIRECTION('',(0.,1.,0.));
#8280=DIRECTION('',(0.,0.,1.));
#8281=DIRECTION('center_axis',(0.,-1.,0.));
#8282=DIRECTION('ref_axis',(1.,0.,0.));
#8283=DIRECTION('',(1.,0.,0.));
#8284=DIRECTION('',(1.,0.,0.));
#8285=DIRECTION('',(0.,0.,1.));
#8286=DIRECTION('center_axis',(-1.,0.,0.));
#8287=DIRECTION('ref_axis',(0.,-1.,0.));
#8288=DIRECTION('',(0.,-1.,0.));
#8289=DIRECTION('',(0.,-1.,0.));
#8290=DIRECTION('center_axis',(0.,0.,1.));
#8291=DIRECTION('ref_axis',(1.,0.,0.));
#8292=DIRECTION('center_axis',(0.,0.,1.));
#8293=DIRECTION('ref_axis',(1.,0.,0.));
#8294=DIRECTION('axis',(0.,0.,1.));
#8295=DIRECTION('refdir',(1.,0.,0.));
#8296=DIRECTION('center_axis',(0.,1.,0.));
#8297=DIRECTION('ref_axis',(-1.,0.,0.));
#8298=DIRECTION('',(-1.,0.,0.));
#8299=DIRECTION('',(0.,0.,1.));
#8300=DIRECTION('',(-1.,0.,0.));
#8301=DIRECTION('',(0.,0.,1.));
#8302=DIRECTION('center_axis',(1.,0.,0.));
#8303=DIRECTION('ref_axis',(0.,1.,0.));
#8304=DIRECTION('',(0.,1.,0.));
#8305=DIRECTION('',(0.,1.,0.));
#8306=DIRECTION('',(0.,0.,1.));
#8307=DIRECTION('center_axis',(0.,-1.,0.));
#8308=DIRECTION('ref_axis',(1.,0.,0.));
#8309=DIRECTION('',(1.,0.,0.));
#8310=DIRECTION('',(1.,0.,0.));
#8311=DIRECTION('',(0.,0.,1.));
#8312=DIRECTION('center_axis',(-1.,0.,0.));
#8313=DIRECTION('ref_axis',(0.,-1.,0.));
#8314=DIRECTION('',(0.,-1.,0.));
#8315=DIRECTION('',(0.,-1.,0.));
#8316=DIRECTION('center_axis',(0.,0.,1.));
#8317=DIRECTION('ref_axis',(1.,0.,0.));
#8318=DIRECTION('center_axis',(0.,0.,1.));
#8319=DIRECTION('ref_axis',(1.,0.,0.));
#8320=DIRECTION('axis',(0.,0.,1.));
#8321=DIRECTION('refdir',(1.,0.,0.));
#8322=DIRECTION('center_axis',(0.,1.,0.));
#8323=DIRECTION('ref_axis',(-1.,0.,0.));
#8324=DIRECTION('',(-1.,0.,0.));
#8325=DIRECTION('',(0.,0.,1.));
#8326=DIRECTION('',(-1.,0.,0.));
#8327=DIRECTION('',(0.,0.,1.));
#8328=DIRECTION('center_axis',(1.,0.,0.));
#8329=DIRECTION('ref_axis',(0.,1.,0.));
#8330=DIRECTION('',(0.,1.,0.));
#8331=DIRECTION('',(0.,1.,0.));
#8332=DIRECTION('',(0.,0.,1.));
#8333=DIRECTION('center_axis',(0.,-1.,0.));
#8334=DIRECTION('ref_axis',(1.,0.,0.));
#8335=DIRECTION('',(1.,0.,0.));
#8336=DIRECTION('',(1.,0.,0.));
#8337=DIRECTION('',(0.,0.,1.));
#8338=DIRECTION('center_axis',(-1.,0.,0.));
#8339=DIRECTION('ref_axis',(0.,-1.,0.));
#8340=DIRECTION('',(0.,-1.,0.));
#8341=DIRECTION('',(0.,-1.,0.));
#8342=DIRECTION('center_axis',(0.,0.,1.));
#8343=DIRECTION('ref_axis',(1.,0.,0.));
#8344=DIRECTION('center_axis',(0.,0.,1.));
#8345=DIRECTION('ref_axis',(1.,0.,0.));
#8346=DIRECTION('axis',(0.,0.,1.));
#8347=DIRECTION('refdir',(1.,0.,0.));
#8348=DIRECTION('center_axis',(0.,0.,1.));
#8349=DIRECTION('ref_axis',(1.,0.,0.));
#8350=DIRECTION('center_axis',(0.,0.,1.));
#8351=DIRECTION('ref_axis',(1.,0.,0.));
#8352=DIRECTION('',(0.,0.,1.));
#8353=DIRECTION('center_axis',(0.,0.,-1.));
#8354=DIRECTION('ref_axis',(1.,0.,0.));
#8355=DIRECTION('center_axis',(0.,1.,0.));
#8356=DIRECTION('ref_axis',(-1.,0.,0.));
#8357=DIRECTION('',(-1.,0.,0.));
#8358=DIRECTION('',(0.,0.,1.));
#8359=DIRECTION('',(-1.,0.,0.));
#8360=DIRECTION('',(0.,0.,1.));
#8361=DIRECTION('center_axis',(1.,0.,0.));
#8362=DIRECTION('ref_axis',(0.,1.,0.));
#8363=DIRECTION('',(0.,1.,0.));
#8364=DIRECTION('',(0.,1.,0.));
#8365=DIRECTION('',(0.,0.,1.));
#8366=DIRECTION('center_axis',(0.,-1.,0.));
#8367=DIRECTION('ref_axis',(1.,0.,0.));
#8368=DIRECTION('',(1.,0.,0.));
#8369=DIRECTION('',(1.,0.,0.));
#8370=DIRECTION('',(0.,0.,1.));
#8371=DIRECTION('center_axis',(-1.,0.,0.));
#8372=DIRECTION('ref_axis',(0.,-1.,0.));
#8373=DIRECTION('',(0.,-1.,0.));
#8374=DIRECTION('',(0.,-1.,0.));
#8375=DIRECTION('center_axis',(0.,0.,1.));
#8376=DIRECTION('ref_axis',(1.,0.,0.));
#8377=DIRECTION('center_axis',(0.,0.,1.));
#8378=DIRECTION('ref_axis',(1.,0.,0.));
#8379=DIRECTION('axis',(0.,0.,1.));
#8380=DIRECTION('refdir',(1.,0.,0.));
#8381=DIRECTION('center_axis',(1.,0.,0.));
#8382=DIRECTION('ref_axis',(0.,0.,-1.));
#8383=DIRECTION('center_axis',(1.,0.,0.));
#8384=DIRECTION('ref_axis',(0.,0.,-1.));
#8385=DIRECTION('',(1.,0.,0.));
#8386=DIRECTION('center_axis',(-1.,0.,0.));
#8387=DIRECTION('ref_axis',(0.,0.,-1.));
#8388=DIRECTION('center_axis',(1.,0.,0.));
#8389=DIRECTION('ref_axis',(0.,0.,-1.));
#8390=DIRECTION('center_axis',(1.,0.,0.));
#8391=DIRECTION('ref_axis',(0.,0.,-1.));
#8392=DIRECTION('',(1.,0.,0.));
#8393=DIRECTION('center_axis',(-1.,0.,0.));
#8394=DIRECTION('ref_axis',(0.,0.,-1.));
#8395=DIRECTION('center_axis',(1.,0.,0.));
#8396=DIRECTION('ref_axis',(0.,0.,-1.));
#8397=DIRECTION('center_axis',(1.,0.,0.));
#8398=DIRECTION('ref_axis',(0.,0.,-1.));
#8399=DIRECTION('',(1.,0.,0.));
#8400=DIRECTION('center_axis',(-1.,0.,0.));
#8401=DIRECTION('ref_axis',(0.,0.,-1.));
#8402=DIRECTION('center_axis',(1.,0.,0.));
#8403=DIRECTION('ref_axis',(0.,0.,-1.));
#8404=DIRECTION('center_axis',(1.,0.,0.));
#8405=DIRECTION('ref_axis',(0.,0.,-1.));
#8406=DIRECTION('',(1.,0.,0.));
#8407=DIRECTION('center_axis',(-1.,0.,0.));
#8408=DIRECTION('ref_axis',(0.,0.,-1.));
#8409=DIRECTION('center_axis',(1.,0.,0.));
#8410=DIRECTION('ref_axis',(0.,0.,-1.));
#8411=DIRECTION('center_axis',(1.,0.,0.));
#8412=DIRECTION('ref_axis',(0.,0.,-1.));
#8413=DIRECTION('',(1.,0.,0.));
#8414=DIRECTION('center_axis',(-1.,0.,0.));
#8415=DIRECTION('ref_axis',(0.,0.,-1.));
#8416=DIRECTION('center_axis',(1.,0.,0.));
#8417=DIRECTION('ref_axis',(0.,0.,-1.));
#8418=DIRECTION('center_axis',(1.,0.,0.));
#8419=DIRECTION('ref_axis',(0.,0.,-1.));
#8420=DIRECTION('',(1.,0.,0.));
#8421=DIRECTION('center_axis',(-1.,0.,0.));
#8422=DIRECTION('ref_axis',(0.,0.,-1.));
#8423=DIRECTION('center_axis',(1.,0.,0.));
#8424=DIRECTION('ref_axis',(0.,0.,-1.));
#8425=DIRECTION('center_axis',(1.,0.,0.));
#8426=DIRECTION('ref_axis',(0.,0.,-1.));
#8427=DIRECTION('',(1.,0.,0.));
#8428=DIRECTION('center_axis',(-1.,0.,0.));
#8429=DIRECTION('ref_axis',(0.,0.,-1.));
#8430=DIRECTION('center_axis',(1.,0.,0.));
#8431=DIRECTION('ref_axis',(0.,0.,-1.));
#8432=DIRECTION('center_axis',(1.,0.,0.));
#8433=DIRECTION('ref_axis',(0.,0.,-1.));
#8434=DIRECTION('',(1.,0.,0.));
#8435=DIRECTION('center_axis',(-1.,0.,0.));
#8436=DIRECTION('ref_axis',(0.,0.,-1.));
#8437=DIRECTION('center_axis',(0.,0.,1.));
#8438=DIRECTION('ref_axis',(0.,-1.,0.));
#8439=DIRECTION('',(0.,1.,0.));
#8440=DIRECTION('',(1.,0.,0.));
#8441=DIRECTION('',(0.,-1.,0.));
#8442=DIRECTION('',(-1.,0.,0.));
#8443=DIRECTION('center_axis',(0.,0.,-1.));
#8444=DIRECTION('ref_axis',(0.,1.,0.));
#8445=DIRECTION('',(0.,-1.,0.));
#8446=DIRECTION('',(1.,0.,0.));
#8447=DIRECTION('',(0.,1.,0.));
#8448=DIRECTION('',(1.,0.,0.));
#8449=DIRECTION('center_axis',(0.,-1.,0.));
#8450=DIRECTION('ref_axis',(0.,0.,-1.));
#8451=DIRECTION('',(0.,0.,1.));
#8452=DIRECTION('',(0.,0.,-1.));
#8453=DIRECTION('center_axis',(-1.,0.,0.));
#8454=DIRECTION('ref_axis',(0.,-1.,0.));
#8455=DIRECTION('',(0.,0.,1.));
#8456=DIRECTION('',(0.,-1.,0.));
#8457=DIRECTION('',(0.,0.,1.));
#8458=DIRECTION('',(0.,-1.,0.));
#8459=DIRECTION('',(0.,0.,1.));
#8460=DIRECTION('center_axis',(0.,1.,0.));
#8461=DIRECTION('ref_axis',(-1.,0.,0.));
#8462=DIRECTION('',(0.,0.,1.));
#8463=DIRECTION('',(-1.,0.,0.));
#8464=DIRECTION('center_axis',(0.,1.,0.));
#8465=DIRECTION('ref_axis',(-1.,0.,0.));
#8466=DIRECTION('',(-1.,0.,0.));
#8467=DIRECTION('',(0.,0.,1.));
#8468=DIRECTION('center_axis',(1.,0.,0.));
#8469=DIRECTION('ref_axis',(0.,1.,0.));
#8470=DIRECTION('',(0.,1.,0.));
#8471=DIRECTION('',(0.,0.,1.));
#8472=DIRECTION('',(0.,1.,0.));
#8473=DIRECTION('center_axis',(0.,-1.,0.));
#8474=DIRECTION('ref_axis',(1.,0.,0.));
#8475=DIRECTION('',(1.,0.,0.));
#8476=DIRECTION('',(1.,0.,0.));
#8477=DIRECTION('center_axis',(0.,0.,1.));
#8478=DIRECTION('ref_axis',(1.,0.,0.));
#8479=DIRECTION('center_axis',(0.,0.,1.));
#8480=DIRECTION('ref_axis',(1.,0.,0.));
#8481=DIRECTION('axis',(0.,0.,1.));
#8482=DIRECTION('refdir',(1.,0.,0.));
#8483=DIRECTION('center_axis',(1.,0.,0.));
#8484=DIRECTION('ref_axis',(0.,0.,-1.));
#8485=DIRECTION('center_axis',(1.,0.,0.));
#8486=DIRECTION('ref_axis',(0.,0.,-1.));
#8487=DIRECTION('',(1.,0.,0.));
#8488=DIRECTION('center_axis',(-1.,0.,0.));
#8489=DIRECTION('ref_axis',(0.,0.,-1.));
#8490=DIRECTION('center_axis',(0.,1.,0.));
#8491=DIRECTION('ref_axis',(-1.,0.,0.));
#8492=DIRECTION('',(-1.,0.,0.));
#8493=DIRECTION('',(0.,0.,1.));
#8494=DIRECTION('',(-1.,0.,0.));
#8495=DIRECTION('',(0.,0.,1.));
#8496=DIRECTION('center_axis',(1.,0.,0.));
#8497=DIRECTION('ref_axis',(0.,1.,0.));
#8498=DIRECTION('',(0.,1.,0.));
#8499=DIRECTION('',(0.,1.,0.));
#8500=DIRECTION('',(0.,0.,1.));
#8501=DIRECTION('center_axis',(0.,-1.,0.));
#8502=DIRECTION('ref_axis',(1.,0.,0.));
#8503=DIRECTION('',(1.,0.,0.));
#8504=DIRECTION('',(1.,0.,0.));
#8505=DIRECTION('',(0.,0.,1.));
#8506=DIRECTION('center_axis',(-1.,0.,0.));
#8507=DIRECTION('ref_axis',(0.,-1.,0.));
#8508=DIRECTION('',(0.,-1.,0.));
#8509=DIRECTION('',(0.,-1.,0.));
#8510=DIRECTION('center_axis',(0.,0.,1.));
#8511=DIRECTION('ref_axis',(1.,0.,0.));
#8512=DIRECTION('center_axis',(0.,0.,1.));
#8513=DIRECTION('ref_axis',(1.,0.,0.));
#8514=DIRECTION('axis',(0.,0.,1.));
#8515=DIRECTION('refdir',(1.,0.,0.));
#8516=DIRECTION('center_axis',(1.,0.,0.));
#8517=DIRECTION('ref_axis',(0.,0.,-1.));
#8518=DIRECTION('center_axis',(1.,0.,0.));
#8519=DIRECTION('ref_axis',(0.,0.,-1.));
#8520=DIRECTION('',(1.,0.,0.));
#8521=DIRECTION('center_axis',(-1.,0.,0.));
#8522=DIRECTION('ref_axis',(0.,0.,-1.));
#8523=DIRECTION('center_axis',(0.,1.,0.));
#8524=DIRECTION('ref_axis',(-1.,0.,0.));
#8525=DIRECTION('',(-1.,0.,0.));
#8526=DIRECTION('',(0.,0.,1.));
#8527=DIRECTION('',(-1.,0.,0.));
#8528=DIRECTION('',(0.,0.,1.));
#8529=DIRECTION('center_axis',(1.,0.,0.));
#8530=DIRECTION('ref_axis',(0.,1.,0.));
#8531=DIRECTION('',(0.,1.,0.));
#8532=DIRECTION('',(0.,1.,0.));
#8533=DIRECTION('',(0.,0.,1.));
#8534=DIRECTION('center_axis',(0.,-1.,0.));
#8535=DIRECTION('ref_axis',(1.,0.,0.));
#8536=DIRECTION('',(1.,0.,0.));
#8537=DIRECTION('',(1.,0.,0.));
#8538=DIRECTION('',(0.,0.,1.));
#8539=DIRECTION('center_axis',(-1.,0.,0.));
#8540=DIRECTION('ref_axis',(0.,-1.,0.));
#8541=DIRECTION('',(0.,-1.,0.));
#8542=DIRECTION('',(0.,-1.,0.));
#8543=DIRECTION('center_axis',(0.,0.,1.));
#8544=DIRECTION('ref_axis',(1.,0.,0.));
#8545=DIRECTION('center_axis',(0.,0.,1.));
#8546=DIRECTION('ref_axis',(1.,0.,0.));
#8547=DIRECTION('axis',(0.,0.,1.));
#8548=DIRECTION('refdir',(1.,0.,0.));
#8549=DIRECTION('center_axis',(0.,0.,1.));
#8550=DIRECTION('ref_axis',(1.,0.,0.));
#8551=DIRECTION('center_axis',(0.,0.,1.));
#8552=DIRECTION('ref_axis',(1.,0.,0.));
#8553=DIRECTION('',(0.,0.,1.));
#8554=DIRECTION('center_axis',(0.,0.,-1.));
#8555=DIRECTION('ref_axis',(1.,0.,0.));
#8556=DIRECTION('center_axis',(0.,0.,1.));
#8557=DIRECTION('ref_axis',(1.,0.,0.));
#8558=DIRECTION('center_axis',(0.,0.,1.));
#8559=DIRECTION('ref_axis',(1.,0.,0.));
#8560=DIRECTION('',(0.,0.,1.));
#8561=DIRECTION('center_axis',(0.,0.,-1.));
#8562=DIRECTION('ref_axis',(1.,0.,0.));
#8563=DIRECTION('center_axis',(0.,0.,1.));
#8564=DIRECTION('ref_axis',(1.,0.,0.));
#8565=DIRECTION('center_axis',(0.,0.,-1.));
#8566=DIRECTION('ref_axis',(1.,0.,0.));
#8567=DIRECTION('',(0.,0.,-1.));
#8568=DIRECTION('center_axis',(0.,0.,1.));
#8569=DIRECTION('ref_axis',(1.,0.,0.));
#8570=DIRECTION('center_axis',(0.,0.,1.));
#8571=DIRECTION('ref_axis',(1.,0.,0.));
#8572=DIRECTION('center_axis',(0.,0.,1.));
#8573=DIRECTION('ref_axis',(1.,0.,0.));
#8574=DIRECTION('',(0.,0.,-1.));
#8575=DIRECTION('center_axis',(0.,0.,-1.));
#8576=DIRECTION('ref_axis',(1.,0.,0.));
#8577=DIRECTION('center_axis',(0.,0.,1.));
#8578=DIRECTION('ref_axis',(1.,0.,0.));
#8579=DIRECTION('center_axis',(0.,0.,1.));
#8580=DIRECTION('ref_axis',(1.,0.,0.));
#8581=DIRECTION('center_axis',(0.,0.,1.));
#8582=DIRECTION('ref_axis',(1.,0.,0.));
#8583=DIRECTION('center_axis',(0.,0.,1.));
#8584=DIRECTION('ref_axis',(1.,0.,0.));
#8585=DIRECTION('',(0.,0.,-1.));
#8586=DIRECTION('center_axis',(0.,0.,1.));
#8587=DIRECTION('ref_axis',(1.,0.,0.));
#8588=DIRECTION('center_axis',(0.,0.,1.));
#8589=DIRECTION('ref_axis',(1.,0.,0.));
#8590=DIRECTION('center_axis',(0.,0.,1.));
#8591=DIRECTION('ref_axis',(1.,0.,0.));
#8592=DIRECTION('axis',(0.,0.,1.));
#8593=DIRECTION('refdir',(1.,0.,0.));
#8594=DIRECTION('center_axis',(0.,0.,1.));
#8595=DIRECTION('ref_axis',(1.,0.,0.));
#8596=DIRECTION('center_axis',(0.,0.,-1.));
#8597=DIRECTION('ref_axis',(1.,0.,0.));
#8598=DIRECTION('',(0.,0.,-1.));
#8599=DIRECTION('center_axis',(0.,0.,-1.));
#8600=DIRECTION('ref_axis',(1.,0.,0.));
#8601=DIRECTION('center_axis',(0.,0.,1.));
#8602=DIRECTION('ref_axis',(1.,0.,0.));
#8603=DIRECTION('center_axis',(0.,0.,1.));
#8604=DIRECTION('ref_axis',(1.,0.,0.));
#8605=DIRECTION('',(0.,0.,-1.));
#8606=DIRECTION('center_axis',(0.,0.,1.));
#8607=DIRECTION('ref_axis',(1.,0.,0.));
#8608=DIRECTION('center_axis',(0.,0.,1.));
#8609=DIRECTION('ref_axis',(1.,0.,0.));
#8610=DIRECTION('center_axis',(0.,0.,1.));
#8611=DIRECTION('ref_axis',(1.,0.,0.));
#8612=DIRECTION('axis',(0.,0.,1.));
#8613=DIRECTION('refdir',(1.,0.,0.));
#8614=DIRECTION('center_axis',(0.,0.,1.));
#8615=DIRECTION('ref_axis',(1.,0.,0.));
#8616=DIRECTION('center_axis',(0.,0.,1.));
#8617=DIRECTION('ref_axis',(1.,0.,0.));
#8618=DIRECTION('',(0.,0.,1.));
#8619=DIRECTION('center_axis',(0.,0.,-1.));
#8620=DIRECTION('ref_axis',(1.,0.,0.));
#8621=DIRECTION('center_axis',(0.,0.,1.));
#8622=DIRECTION('ref_axis',(1.,0.,0.));
#8623=DIRECTION('center_axis',(0.,0.,1.));
#8624=DIRECTION('ref_axis',(1.,0.,0.));
#8625=DIRECTION('',(0.,0.,1.));
#8626=DIRECTION('center_axis',(0.,0.,-1.));
#8627=DIRECTION('ref_axis',(1.,0.,0.));
#8628=DIRECTION('center_axis',(0.,0.,1.));
#8629=DIRECTION('ref_axis',(1.,0.,0.));
#8630=DIRECTION('center_axis',(0.,0.,1.));
#8631=DIRECTION('ref_axis',(1.,0.,0.));
#8632=DIRECTION('',(0.,0.,1.));
#8633=DIRECTION('center_axis',(0.,0.,-1.));
#8634=DIRECTION('ref_axis',(1.,0.,0.));
#8635=DIRECTION('center_axis',(0.,0.,1.));
#8636=DIRECTION('ref_axis',(1.,0.,0.));
#8637=DIRECTION('center_axis',(0.,0.,1.));
#8638=DIRECTION('ref_axis',(1.,0.,0.));
#8639=DIRECTION('center_axis',(0.,0.,1.));
#8640=DIRECTION('ref_axis',(1.,0.,0.));
#8641=DIRECTION('center_axis',(0.,0.,1.));
#8642=DIRECTION('ref_axis',(1.,0.,0.));
#8643=DIRECTION('',(0.,0.,-1.));
#8644=DIRECTION('center_axis',(0.,0.,1.));
#8645=DIRECTION('ref_axis',(1.,0.,0.));
#8646=DIRECTION('center_axis',(0.,0.,1.));
#8647=DIRECTION('ref_axis',(1.,0.,0.));
#8648=DIRECTION('center_axis',(0.,0.,-1.));
#8649=DIRECTION('ref_axis',(1.,0.,0.));
#8650=DIRECTION('center_axis',(0.,0.,1.));
#8651=DIRECTION('ref_axis',(1.,0.,0.));
#8652=DIRECTION('',(0.,0.,-1.));
#8653=DIRECTION('center_axis',(0.,0.,1.));
#8654=DIRECTION('ref_axis',(1.,0.,0.));
#8655=DIRECTION('center_axis',(0.,0.,1.));
#8656=DIRECTION('ref_axis',(1.,0.,0.));
#8657=DIRECTION('',(0.,0.,-1.));
#8658=DIRECTION('center_axis',(0.,0.,1.));
#8659=DIRECTION('ref_axis',(1.,0.,0.));
#8660=DIRECTION('center_axis',(0.,0.,1.));
#8661=DIRECTION('ref_axis',(1.,0.,0.));
#8662=DIRECTION('center_axis',(0.,0.,1.));
#8663=DIRECTION('ref_axis',(1.,0.,0.));
#8664=DIRECTION('axis',(0.,0.,1.));
#8665=DIRECTION('refdir',(1.,0.,0.));
#8666=DIRECTION('center_axis',(0.,0.,1.));
#8667=DIRECTION('ref_axis',(1.,0.,0.));
#8668=DIRECTION('center_axis',(0.,0.,1.));
#8669=DIRECTION('ref_axis',(1.,0.,0.));
#8670=DIRECTION('center_axis',(0.,0.,1.));
#8671=DIRECTION('ref_axis',(1.,0.,0.));
#8672=DIRECTION('center_axis',(0.,0.,1.));
#8673=DIRECTION('ref_axis',(1.,0.,0.));
#8674=DIRECTION('center_axis',(0.,0.,1.));
#8675=DIRECTION('ref_axis',(1.,0.,0.));
#8676=DIRECTION('center_axis',(0.,0.,-1.));
#8677=DIRECTION('ref_axis',(1.,0.,0.));
#8678=DIRECTION('center_axis',(0.,0.,1.));
#8679=DIRECTION('ref_axis',(1.,0.,0.));
#8680=DIRECTION('',(0.,0.,-1.));
#8681=DIRECTION('center_axis',(0.,0.,1.));
#8682=DIRECTION('ref_axis',(1.,0.,0.));
#8683=DIRECTION('',(0.,0.,-1.));
#8684=DIRECTION('center_axis',(0.,0.,1.));
#8685=DIRECTION('ref_axis',(1.,0.,0.));
#8686=DIRECTION('center_axis',(0.,0.,1.));
#8687=DIRECTION('ref_axis',(1.,0.,0.));
#8688=DIRECTION('center_axis',(0.,0.,1.));
#8689=DIRECTION('ref_axis',(1.,0.,0.));
#8690=DIRECTION('',(0.,0.,-1.));
#8691=DIRECTION('center_axis',(0.,0.,1.));
#8692=DIRECTION('ref_axis',(1.,0.,0.));
#8693=DIRECTION('center_axis',(0.,0.,1.));
#8694=DIRECTION('ref_axis',(1.,0.,0.));
#8695=DIRECTION('axis',(0.,0.,1.));
#8696=DIRECTION('refdir',(1.,0.,0.));
#8697=DIRECTION('center_axis',(0.,0.,1.));
#8698=DIRECTION('ref_axis',(1.,0.,0.));
#8699=DIRECTION('center_axis',(0.,0.,-1.));
#8700=DIRECTION('ref_axis',(1.,0.,0.));
#8701=DIRECTION('',(0.,0.,-1.));
#8702=DIRECTION('center_axis',(0.,0.,-1.));
#8703=DIRECTION('ref_axis',(1.,0.,0.));
#8704=DIRECTION('center_axis',(0.,0.,1.));
#8705=DIRECTION('ref_axis',(1.,0.,0.));
#8706=DIRECTION('center_axis',(0.,0.,1.));
#8707=DIRECTION('ref_axis',(1.,0.,0.));
#8708=DIRECTION('',(0.,0.,-1.));
#8709=DIRECTION('center_axis',(0.,0.,1.));
#8710=DIRECTION('ref_axis',(1.,0.,0.));
#8711=DIRECTION('center_axis',(0.,0.,1.));
#8712=DIRECTION('ref_axis',(1.,0.,0.));
#8713=DIRECTION('center_axis',(0.,0.,1.));
#8714=DIRECTION('ref_axis',(1.,0.,0.));
#8715=DIRECTION('axis',(0.,0.,1.));
#8716=DIRECTION('refdir',(1.,0.,0.));
#8717=DIRECTION('center_axis',(0.,0.,1.));
#8718=DIRECTION('ref_axis',(1.,0.,0.));
#8719=DIRECTION('center_axis',(0.,0.,1.));
#8720=DIRECTION('ref_axis',(1.,0.,0.));
#8721=DIRECTION('center_axis',(0.,0.,1.));
#8722=DIRECTION('ref_axis',(1.,0.,0.));
#8723=DIRECTION('center_axis',(0.,0.,1.));
#8724=DIRECTION('ref_axis',(1.,0.,0.));
#8725=DIRECTION('center_axis',(0.,0.,1.));
#8726=DIRECTION('ref_axis',(1.,0.,0.));
#8727=DIRECTION('center_axis',(0.,0.,-1.));
#8728=DIRECTION('ref_axis',(1.,0.,0.));
#8729=DIRECTION('center_axis',(0.,0.,1.));
#8730=DIRECTION('ref_axis',(1.,0.,0.));
#8731=DIRECTION('',(0.,0.,-1.));
#8732=DIRECTION('center_axis',(0.,0.,1.));
#8733=DIRECTION('ref_axis',(1.,0.,0.));
#8734=DIRECTION('',(0.,0.,-1.));
#8735=DIRECTION('center_axis',(0.,0.,1.));
#8736=DIRECTION('ref_axis',(1.,0.,0.));
#8737=DIRECTION('center_axis',(0.,0.,1.));
#8738=DIRECTION('ref_axis',(1.,0.,0.));
#8739=DIRECTION('center_axis',(0.,0.,1.));
#8740=DIRECTION('ref_axis',(1.,0.,0.));
#8741=DIRECTION('',(0.,0.,-1.));
#8742=DIRECTION('center_axis',(0.,0.,1.));
#8743=DIRECTION('ref_axis',(1.,0.,0.));
#8744=DIRECTION('center_axis',(0.,0.,1.));
#8745=DIRECTION('ref_axis',(1.,0.,0.));
#8746=DIRECTION('axis',(0.,0.,1.));
#8747=DIRECTION('refdir',(1.,0.,0.));
#8748=DIRECTION('center_axis',(0.,0.,1.));
#8749=DIRECTION('ref_axis',(1.,0.,0.));
#8750=DIRECTION('center_axis',(0.,0.,-1.));
#8751=DIRECTION('ref_axis',(1.,0.,0.));
#8752=DIRECTION('',(0.,0.,-1.));
#8753=DIRECTION('center_axis',(0.,0.,-1.));
#8754=DIRECTION('ref_axis',(1.,0.,0.));
#8755=DIRECTION('center_axis',(0.,0.,1.));
#8756=DIRECTION('ref_axis',(1.,0.,0.));
#8757=DIRECTION('center_axis',(0.,0.,1.));
#8758=DIRECTION('ref_axis',(1.,0.,0.));
#8759=DIRECTION('',(0.,0.,-1.));
#8760=DIRECTION('center_axis',(0.,0.,1.));
#8761=DIRECTION('ref_axis',(1.,0.,0.));
#8762=DIRECTION('center_axis',(0.,0.,1.));
#8763=DIRECTION('ref_axis',(1.,0.,0.));
#8764=DIRECTION('center_axis',(0.,0.,1.));
#8765=DIRECTION('ref_axis',(1.,0.,0.));
#8766=DIRECTION('axis',(0.,0.,1.));
#8767=DIRECTION('refdir',(1.,0.,0.));
#8768=DIRECTION('center_axis',(-0.00013439580876317,0.999252824179506,0.0386493894783381));
#8769=DIRECTION('ref_axis',(5.19819987946072E-6,-0.0386493891287688,0.999252833217375));
#8770=DIRECTION('center_axis',(0.000134396360781948,0.999252824161965,0.0386493899299144));
#8771=DIRECTION('ref_axis',(0.987395345410578,-0.00624976689623724,0.158149841211642));
#8772=DIRECTION('center_axis',(0.000134396360781948,0.999252824161965,0.0386493899299144));
#8773=DIRECTION('ref_axis',(0.987395345410578,-0.00624976689623724,0.158149841211642));
#8774=DIRECTION('center_axis',(-0.00013439580876317,0.999252824179506,0.0386493894783381));
#8775=DIRECTION('ref_axis',(5.19819987946073E-6,-0.0386493891287688,0.999252833217375));
#8776=DIRECTION('axis',(0.,0.,1.));
#8777=DIRECTION('refdir',(1.,0.,0.));
#8778=DIRECTION('center_axis',(0.,1.,0.));
#8779=DIRECTION('ref_axis',(-1.83697019872103E-16,0.,-1.));
#8780=DIRECTION('center_axis',(0.,0.916157334902189,-0.400818834019708));
#8781=DIRECTION('ref_axis',(0.,-0.400818834019708,-0.916157334902189));
#8782=DIRECTION('center_axis',(0.,1.,0.));
#8783=DIRECTION('ref_axis',(1.,0.,0.));
#8784=DIRECTION('center_axis',(0.,1.,0.));
#8785=DIRECTION('ref_axis',(1.,0.,0.));
#8786=DIRECTION('',(1.,0.,0.));
#8787=DIRECTION('center_axis',(0.,-1.,0.));
#8788=DIRECTION('ref_axis',(1.,0.,0.));
#8789=DIRECTION('center_axis',(0.,-1.,0.));
#8790=DIRECTION('ref_axis',(1.,0.,0.));
#8791=DIRECTION('',(1.,0.,0.));
#8792=DIRECTION('center_axis',(0.,-0.916157334902189,0.400818834019708));
#8793=DIRECTION('ref_axis',(0.,-0.400818834019708,-0.916157334902189));
#8794=DIRECTION('',(0.,0.400818834019708,0.916157334902189));
#8795=DIRECTION('',(1.,0.,0.));
#8796=DIRECTION('',(0.,-0.400818834019708,-0.916157334902189));
#8797=DIRECTION('',(1.,0.,0.));
#8798=DIRECTION('center_axis',(0.,0.916157334902189,-0.400818834019708));
#8799=DIRECTION('ref_axis',(0.,0.400818834019708,0.916157334902189));
#8800=DIRECTION('',(-1.,0.,0.));
#8801=DIRECTION('center_axis',(0.,0.916157334902189,-0.400818834019708));
#8802=DIRECTION('ref_axis',(0.,-0.400818834019708,-0.916157334902189));
#8803=DIRECTION('center_axis',(0.,1.,0.));
#8804=DIRECTION('ref_axis',(1.,0.,0.));
#8805=DIRECTION('',(0.,1.,0.));
#8806=DIRECTION('center_axis',(0.,-1.,0.));
#8807=DIRECTION('ref_axis',(1.,0.,0.));
#8808=DIRECTION('center_axis',(0.,0.,1.));
#8809=DIRECTION('ref_axis',(1.,0.,0.));
#8810=DIRECTION('center_axis',(0.,0.,1.));
#8811=DIRECTION('ref_axis',(1.,0.,0.));
#8812=DIRECTION('center_axis',(0.,0.,1.));
#8813=DIRECTION('ref_axis',(1.,0.,0.));
#8814=DIRECTION('center_axis',(0.,0.,1.));
#8815=DIRECTION('ref_axis',(6.12323399573677E-17,1.,0.));
#8816=DIRECTION('center_axis',(0.,0.,1.));
#8817=DIRECTION('ref_axis',(1.,0.,0.));
#8818=DIRECTION('center_axis',(0.,0.,1.));
#8819=DIRECTION('ref_axis',(1.,0.,0.));
#8820=DIRECTION('',(0.,0.,1.));
#8821=DIRECTION('center_axis',(0.,1.,0.));
#8822=DIRECTION('ref_axis',(0.,0.,1.));
#8823=DIRECTION('',(0.,0.,-1.));
#8824=DIRECTION('',(0.,0.,1.));
#8825=DIRECTION('',(1.,0.,0.));
#8826=DIRECTION('center_axis',(0.,0.,-1.));
#8827=DIRECTION('ref_axis',(0.,1.,0.));
#8828=DIRECTION('',(0.,-1.,0.));
#8829=DIRECTION('',(0.,1.,0.));
#8830=DIRECTION('center_axis',(1.,0.,0.));
#8831=DIRECTION('ref_axis',(0.,0.,-1.));
#8832=DIRECTION('center_axis',(1.,0.,0.));
#8833=DIRECTION('ref_axis',(0.,0.,-1.));
#8834=DIRECTION('axis',(0.,0.,1.));
#8835=DIRECTION('refdir',(1.,0.,0.));
#8836=DIRECTION('center_axis',(0.,1.,0.));
#8837=DIRECTION('ref_axis',(6.12323399573677E-17,0.,-1.));
#8838=DIRECTION('center_axis',(0.,-0.916157334902189,-0.400818834019708));
#8839=DIRECTION('ref_axis',(0.,0.400818834019708,-0.916157334902189));
#8840=DIRECTION('center_axis',(0.,1.,0.));
#8841=DIRECTION('ref_axis',(1.,0.,0.));
#8842=DIRECTION('center_axis',(0.,1.,0.));
#8843=DIRECTION('ref_axis',(1.,0.,0.));
#8844=DIRECTION('',(-1.,0.,0.));
#8845=DIRECTION('center_axis',(0.,1.,0.));
#8846=DIRECTION('ref_axis',(1.,0.,0.));
#8847=DIRECTION('center_axis',(0.,1.,0.));
#8848=DIRECTION('ref_axis',(1.,0.,0.));
#8849=DIRECTION('',(-1.,0.,0.));
#8850=DIRECTION('center_axis',(0.,0.916157334902189,0.400818834019708));
#8851=DIRECTION('ref_axis',(0.,-0.400818834019708,0.916157334902189));
#8852=DIRECTION('',(0.,-0.400818834019708,0.916157334902189));
#8853=DIRECTION('',(1.,0.,0.));
#8854=DIRECTION('',(0.,-0.400818834019708,0.916157334902189));
#8855=DIRECTION('',(1.,0.,0.));
#8856=DIRECTION('center_axis',(0.,-0.916157334902189,-0.400818834019708));
#8857=DIRECTION('ref_axis',(0.,0.400818834019708,-0.916157334902189));
#8858=DIRECTION('',(1.,0.,0.));
#8859=DIRECTION('center_axis',(0.,-0.916157334902189,-0.400818834019708));
#8860=DIRECTION('ref_axis',(0.,0.400818834019708,-0.916157334902189));
#8861=DIRECTION('center_axis',(0.,1.,0.));
#8862=DIRECTION('ref_axis',(1.,0.,0.));
#8863=DIRECTION('center_axis',(0.,1.,0.));
#8864=DIRECTION('ref_axis',(1.,0.,0.));
#8865=DIRECTION('',(0.,1.,0.));
#8866=DIRECTION('center_axis',(0.,0.,1.));
#8867=DIRECTION('ref_axis',(1.,0.,0.));
#8868=DIRECTION('center_axis',(0.,0.,1.));
#8869=DIRECTION('ref_axis',(1.,0.,0.));
#8870=DIRECTION('center_axis',(0.,0.,1.));
#8871=DIRECTION('ref_axis',(1.,0.,0.));
#8872=DIRECTION('center_axis',(0.,0.,1.));
#8873=DIRECTION('ref_axis',(-1.83697019872103E-16,-1.,0.));
#8874=DIRECTION('center_axis',(0.,0.,1.));
#8875=DIRECTION('ref_axis',(1.,0.,0.));
#8876=DIRECTION('center_axis',(0.,0.,1.));
#8877=DIRECTION('ref_axis',(1.,0.,0.));
#8878=DIRECTION('',(0.,0.,1.));
#8879=DIRECTION('center_axis',(0.,0.,-1.));
#8880=DIRECTION('ref_axis',(0.,1.,0.));
#8881=DIRECTION('',(0.,1.,0.));
#8882=DIRECTION('',(0.,1.,0.));
#8883=DIRECTION('',(1.,0.,0.));
#8884=DIRECTION('center_axis',(0.,-1.,0.));
#8885=DIRECTION('ref_axis',(0.,0.,-1.));
#8886=DIRECTION('',(0.,0.,-1.));
#8887=DIRECTION('',(0.,0.,-1.));
#8888=DIRECTION('center_axis',(1.,0.,0.));
#8889=DIRECTION('ref_axis',(0.,0.,-1.));
#8890=DIRECTION('center_axis',(1.,0.,0.));
#8891=DIRECTION('ref_axis',(0.,0.,-1.));
#8892=DIRECTION('axis',(0.,0.,1.));
#8893=DIRECTION('refdir',(1.,0.,0.));
#8894=DIRECTION('center_axis',(0.,0.,-1.));
#8895=DIRECTION('ref_axis',(0.,1.,0.));
#8896=DIRECTION('',(0.,1.,0.));
#8897=DIRECTION('',(1.,0.,0.));
#8898=DIRECTION('',(0.,-1.,0.));
#8899=DIRECTION('',(1.,0.,0.));
#8900=DIRECTION('center_axis',(0.,1.,-8.88178419700125E-16));
#8901=DIRECTION('ref_axis',(0.,8.88178419700125E-16,1.));
#8902=DIRECTION('',(0.,8.88178419700125E-16,1.));
#8903=DIRECTION('',(1.,0.,0.));
#8904=DIRECTION('',(0.,-8.88178419700125E-16,-1.));
#8905=DIRECTION('center_axis',(0.,-7.40148683083439E-16,-1.));
#8906=DIRECTION('ref_axis',(0.,1.,-7.40148683083439E-16));
#8907=DIRECTION('',(0.,1.,-7.40148683083439E-16));
#8908=DIRECTION('',(1.,0.,0.));
#8909=DIRECTION('',(0.,-1.,7.40148683083439E-16));
#8910=DIRECTION('center_axis',(0.,-0.707106781186547,-0.707106781186548));
#8911=DIRECTION('ref_axis',(0.,0.707106781186548,-0.707106781186547));
#8912=DIRECTION('',(0.,0.707106781186548,-0.707106781186547));
#8913=DIRECTION('',(1.,0.,0.));
#8914=DIRECTION('',(0.,-0.707106781186548,0.707106781186547));
#8915=DIRECTION('center_axis',(0.,-1.,2.77555756156289E-16));
#8916=DIRECTION('ref_axis',(0.,-2.77555756156289E-16,-1.));
#8917=DIRECTION('',(0.,-2.77555756156289E-16,-1.));
#8918=DIRECTION('',(1.,0.,0.));
#8919=DIRECTION('',(0.,2.77555756156289E-16,1.));
#8920=DIRECTION('center_axis',(0.,-0.707106781186547,0.707106781186548));
#8921=DIRECTION('ref_axis',(0.,-0.707106781186548,-0.707106781186547));
#8922=DIRECTION('',(0.,-0.707106781186548,-0.707106781186547));
#8923=DIRECTION('',(1.,0.,0.));
#8924=DIRECTION('',(0.,0.707106781186548,0.707106781186547));
#8925=DIRECTION('center_axis',(0.,7.40148683083438E-16,1.));
#8926=DIRECTION('ref_axis',(0.,-1.,7.40148683083438E-16));
#8927=DIRECTION('',(0.,-1.,7.40148683083438E-16));
#8928=DIRECTION('',(1.,0.,0.));
#8929=DIRECTION('',(0.,1.,-7.40148683083438E-16));
#8930=DIRECTION('center_axis',(0.,1.,-4.44089209850063E-16));
#8931=DIRECTION('ref_axis',(0.,4.44089209850063E-16,1.));
#8932=DIRECTION('',(0.,4.44089209850063E-16,1.));
#8933=DIRECTION('',(1.,0.,0.));
#8934=DIRECTION('',(0.,-4.44089209850063E-16,-1.));
#8935=DIRECTION('center_axis',(0.,2.41352831440251E-16,1.));
#8936=DIRECTION('ref_axis',(0.,-1.,2.41352831440251E-16));
#8937=DIRECTION('',(0.,-1.,2.41352831440251E-16));
#8938=DIRECTION('',(-1.,0.,0.));
#8939=DIRECTION('',(0.,1.,-2.41352831440251E-16));
#8940=DIRECTION('center_axis',(0.,-1.,2.41352831440251E-16));
#8941=DIRECTION('ref_axis',(0.,-2.41352831440251E-16,-1.));
#8942=DIRECTION('',(0.,-2.41352831440251E-16,-1.));
#8943=DIRECTION('',(1.,0.,0.));
#8944=DIRECTION('',(0.,2.41352831440251E-16,1.));
#8945=DIRECTION('',(1.,0.,0.));
#8946=DIRECTION('center_axis',(0.,0.,-1.));
#8947=DIRECTION('ref_axis',(0.,1.,0.));
#8948=DIRECTION('',(0.,1.,0.));
#8949=DIRECTION('',(1.,0.,0.));
#8950=DIRECTION('',(0.,-1.,0.));
#8951=DIRECTION('center_axis',(0.,-1.,0.));
#8952=DIRECTION('ref_axis',(0.,0.,-1.));
#8953=DIRECTION('',(0.,0.,-1.));
#8954=DIRECTION('',(1.,0.,0.));
#8955=DIRECTION('',(0.,0.,1.));
#8956=DIRECTION('center_axis',(0.,-0.707106781186547,0.707106781186548));
#8957=DIRECTION('ref_axis',(0.,-0.707106781186548,-0.707106781186547));
#8958=DIRECTION('',(0.,-0.707106781186548,-0.707106781186547));
#8959=DIRECTION('',(1.,0.,0.));
#8960=DIRECTION('',(0.,0.707106781186548,0.707106781186547));
#8961=DIRECTION('center_axis',(0.,0.,1.));
#8962=DIRECTION('ref_axis',(0.,-1.,0.));
#8963=DIRECTION('',(0.,-1.,0.));
#8964=DIRECTION('',(1.,0.,0.));
#8965=DIRECTION('',(0.,1.,0.));
#8966=DIRECTION('center_axis',(0.,0.707106781186548,0.707106781186547));
#8967=DIRECTION('ref_axis',(0.,-0.707106781186547,0.707106781186548));
#8968=DIRECTION('',(0.,-0.707106781186547,0.707106781186548));
#8969=DIRECTION('',(1.,0.,0.));
#8970=DIRECTION('',(0.,0.707106781186547,-0.707106781186548));
#8971=DIRECTION('center_axis',(0.,1.,0.));
#8972=DIRECTION('ref_axis',(0.,0.,1.));
#8973=DIRECTION('',(0.,0.,1.));
#8974=DIRECTION('',(1.,0.,0.));
#8975=DIRECTION('',(0.,0.,-1.));
#8976=DIRECTION('center_axis',(0.,0.,-1.));
#8977=DIRECTION('ref_axis',(0.,1.,0.));
#8978=DIRECTION('',(0.,1.,0.));
#8979=DIRECTION('',(1.,0.,0.));
#8980=DIRECTION('',(0.,-1.,0.));
#8981=DIRECTION('center_axis',(0.,1.,-2.41352831440251E-16));
#8982=DIRECTION('ref_axis',(0.,2.41352831440251E-16,1.));
#8983=DIRECTION('',(0.,2.41352831440251E-16,1.));
#8984=DIRECTION('',(-1.,0.,0.));
#8985=DIRECTION('',(0.,-2.41352831440251E-16,-1.));
#8986=DIRECTION('center_axis',(0.,0.,1.));
#8987=DIRECTION('ref_axis',(0.,-1.,0.));
#8988=DIRECTION('',(0.,-1.,0.));
#8989=DIRECTION('',(1.,0.,0.));
#8990=DIRECTION('',(0.,1.,0.));
#8991=DIRECTION('',(1.,0.,0.));
#8992=DIRECTION('center_axis',(0.,-1.,0.));
#8993=DIRECTION('ref_axis',(0.,0.,-1.));
#8994=DIRECTION('',(0.,0.,-1.));
#8995=DIRECTION('',(1.,0.,0.));
#8996=DIRECTION('',(0.,0.,1.));
#8997=DIRECTION('center_axis',(0.,0.,1.));
#8998=DIRECTION('ref_axis',(0.,-1.,0.));
#8999=DIRECTION('',(0.,-1.,0.));
#9000=DIRECTION('',(1.,0.,0.));
#9001=DIRECTION('',(0.,1.,0.));
#9002=DIRECTION('center_axis',(0.,0.707106781186548,0.707106781186548));
#9003=DIRECTION('ref_axis',(0.,-0.707106781186548,0.707106781186548));
#9004=DIRECTION('',(0.,-0.707106781186548,0.707106781186548));
#9005=DIRECTION('',(1.,0.,0.));
#9006=DIRECTION('',(0.,0.707106781186548,-0.707106781186548));
#9007=DIRECTION('center_axis',(0.,1.,0.));
#9008=DIRECTION('ref_axis',(0.,0.,1.));
#9009=DIRECTION('',(0.,0.,1.));
#9010=DIRECTION('',(1.,0.,0.));
#9011=DIRECTION('',(0.,0.,-1.));
#9012=DIRECTION('center_axis',(0.,0.707106781186548,-0.707106781186547));
#9013=DIRECTION('ref_axis',(0.,0.707106781186547,0.707106781186548));
#9014=DIRECTION('',(0.,0.707106781186547,0.707106781186548));
#9015=DIRECTION('',(1.,0.,0.));
#9016=DIRECTION('',(0.,-0.707106781186547,-0.707106781186548));
#9017=DIRECTION('center_axis',(0.,-7.40148683083438E-16,-1.));
#9018=DIRECTION('ref_axis',(0.,1.,-7.40148683083438E-16));
#9019=DIRECTION('',(0.,1.,-7.40148683083438E-16));
#9020=DIRECTION('',(1.,0.,0.));
#9021=DIRECTION('',(0.,-1.,7.40148683083438E-16));
#9022=DIRECTION('center_axis',(0.,-1.,0.));
#9023=DIRECTION('ref_axis',(0.,0.,-1.));
#9024=DIRECTION('',(0.,0.,-1.));
#9025=DIRECTION('',(1.,0.,0.));
#9026=DIRECTION('',(0.,0.,1.));
#9027=DIRECTION('center_axis',(0.,0.,-1.));
#9028=DIRECTION('ref_axis',(0.,1.,0.));
#9029=DIRECTION('',(0.,1.,0.));
#9030=DIRECTION('',(-1.,0.,0.));
#9031=DIRECTION('',(0.,-1.,0.));
#9032=DIRECTION('center_axis',(0.,1.,0.));
#9033=DIRECTION('ref_axis',(0.,0.,1.));
#9034=DIRECTION('',(0.,0.,1.));
#9035=DIRECTION('',(1.,0.,0.));
#9036=DIRECTION('',(0.,0.,-1.));
#9037=DIRECTION('',(1.,0.,0.));
#9038=DIRECTION('center_axis',(0.,0.,1.));
#9039=DIRECTION('ref_axis',(0.,-1.,0.));
#9040=DIRECTION('',(0.,-1.,0.));
#9041=DIRECTION('',(1.,0.,0.));
#9042=DIRECTION('',(0.,1.,0.));
#9043=DIRECTION('center_axis',(0.,1.,0.));
#9044=DIRECTION('ref_axis',(0.,0.,1.));
#9045=DIRECTION('',(0.,0.,1.));
#9046=DIRECTION('',(1.,0.,0.));
#9047=DIRECTION('',(0.,0.,-1.));
#9048=DIRECTION('center_axis',(0.,0.707106781186547,-0.707106781186548));
#9049=DIRECTION('ref_axis',(0.,0.707106781186548,0.707106781186547));
#9050=DIRECTION('',(0.,0.707106781186548,0.707106781186547));
#9051=DIRECTION('',(1.,0.,0.));
#9052=DIRECTION('',(0.,-0.707106781186548,-0.707106781186547));
#9053=DIRECTION('center_axis',(0.,0.,-1.));
#9054=DIRECTION('ref_axis',(0.,1.,0.));
#9055=DIRECTION('',(0.,1.,0.));
#9056=DIRECTION('',(1.,0.,0.));
#9057=DIRECTION('',(0.,-1.,0.));
#9058=DIRECTION('center_axis',(0.,-0.707106781186547,-0.707106781186548));
#9059=DIRECTION('ref_axis',(0.,0.707106781186548,-0.707106781186547));
#9060=DIRECTION('',(0.,0.707106781186548,-0.707106781186547));
#9061=DIRECTION('',(1.,0.,0.));
#9062=DIRECTION('',(0.,-0.707106781186548,0.707106781186547));
#9063=DIRECTION('center_axis',(0.,-1.,0.));
#9064=DIRECTION('ref_axis',(0.,0.,-1.));
#9065=DIRECTION('',(0.,0.,-1.));
#9066=DIRECTION('',(1.,0.,0.));
#9067=DIRECTION('',(0.,0.,1.));
#9068=DIRECTION('center_axis',(0.,0.,1.));
#9069=DIRECTION('ref_axis',(0.,-1.,0.));
#9070=DIRECTION('',(0.,-1.,0.));
#9071=DIRECTION('',(1.,0.,0.));
#9072=DIRECTION('',(0.,1.,0.));
#9073=DIRECTION('center_axis',(0.,-1.,0.));
#9074=DIRECTION('ref_axis',(0.,0.,-1.));
#9075=DIRECTION('',(0.,0.,-1.));
#9076=DIRECTION('',(-1.,0.,0.));
#9077=DIRECTION('',(0.,0.,1.));
#9078=DIRECTION('center_axis',(1.,0.,0.));
#9079=DIRECTION('ref_axis',(0.,0.,-1.));
#9080=DIRECTION('center_axis',(1.,0.,0.));
#9081=DIRECTION('ref_axis',(0.,0.,-1.));
#9082=DIRECTION('',(1.,0.,0.));
#9083=DIRECTION('center_axis',(-1.,0.,0.));
#9084=DIRECTION('ref_axis',(0.,0.,-1.));
#9085=DIRECTION('center_axis',(0.,1.,0.));
#9086=DIRECTION('ref_axis',(0.,0.,1.));
#9087=DIRECTION('',(0.,0.,1.));
#9088=DIRECTION('',(1.,0.,0.));
#9089=DIRECTION('',(0.,0.,1.));
#9090=DIRECTION('center_axis',(0.,1.,0.));
#9091=DIRECTION('ref_axis',(0.,0.,1.));
#9092=DIRECTION('',(0.,0.,1.));
#9093=DIRECTION('',(1.,0.,0.));
#9094=DIRECTION('',(0.,0.,1.));
#9095=DIRECTION('center_axis',(0.,0.,-1.));
#9096=DIRECTION('ref_axis',(0.,1.,0.));
#9097=DIRECTION('',(0.,1.,0.));
#9098=DIRECTION('',(0.,1.,0.));
#9099=DIRECTION('center_axis',(0.,0.,-1.));
#9100=DIRECTION('ref_axis',(0.,1.,0.));
#9101=DIRECTION('',(0.,1.,0.));
#9102=DIRECTION('',(1.,0.,0.));
#9103=DIRECTION('',(0.,1.,0.));
#9104=DIRECTION('center_axis',(0.,-1.,0.));
#9105=DIRECTION('ref_axis',(0.,0.,-1.));
#9106=DIRECTION('',(0.,0.,-1.));
#9107=DIRECTION('',(0.,0.,-1.));
#9108=DIRECTION('center_axis',(0.,-1.,0.));
#9109=DIRECTION('ref_axis',(0.,0.,-1.));
#9110=DIRECTION('',(0.,0.,-1.));
#9111=DIRECTION('',(1.,0.,0.));
#9112=DIRECTION('',(0.,0.,-1.));
#9113=DIRECTION('center_axis',(0.,0.,1.));
#9114=DIRECTION('ref_axis',(0.,-1.,0.));
#9115=DIRECTION('',(0.,-1.,0.));
#9116=DIRECTION('',(0.,-1.,0.));
#9117=DIRECTION('center_axis',(0.,0.,1.));
#9118=DIRECTION('ref_axis',(0.,-1.,0.));
#9119=DIRECTION('',(0.,-1.,0.));
#9120=DIRECTION('',(0.,-1.,0.));
#9121=DIRECTION('center_axis',(1.,0.,0.));
#9122=DIRECTION('ref_axis',(0.,0.,-1.));
#9123=DIRECTION('center_axis',(1.,0.,0.));
#9124=DIRECTION('ref_axis',(0.,0.,-1.));
#9125=DIRECTION('axis',(0.,0.,1.));
#9126=DIRECTION('refdir',(1.,0.,0.));
#9127=DIRECTION('center_axis',(0.,0.,1.));
#9128=DIRECTION('ref_axis',(1.,0.,0.));
#9129=DIRECTION('center_axis',(0.,0.,1.));
#9130=DIRECTION('ref_axis',(1.,0.,0.));
#9131=DIRECTION('',(0.,0.,1.));
#9132=DIRECTION('center_axis',(0.,0.,-1.));
#9133=DIRECTION('ref_axis',(1.,0.,0.));
#9134=DIRECTION('center_axis',(0.,0.,1.));
#9135=DIRECTION('ref_axis',(1.,0.,0.));
#9136=DIRECTION('center_axis',(0.,0.,1.));
#9137=DIRECTION('ref_axis',(1.,0.,0.));
#9138=DIRECTION('center_axis',(0.,0.,1.));
#9139=DIRECTION('ref_axis',(1.,0.,0.));
#9140=DIRECTION('center_axis',(0.,0.,1.));
#9141=DIRECTION('ref_axis',(1.,0.,0.));
#9142=DIRECTION('',(0.,0.,1.));
#9143=DIRECTION('center_axis',(0.,0.,-1.));
#9144=DIRECTION('ref_axis',(1.,0.,0.));
#9145=DIRECTION('center_axis',(0.,0.,1.));
#9146=DIRECTION('ref_axis',(1.,0.,0.));
#9147=DIRECTION('center_axis',(0.,0.,1.));
#9148=DIRECTION('ref_axis',(1.,0.,0.));
#9149=DIRECTION('center_axis',(0.,0.,1.));
#9150=DIRECTION('ref_axis',(1.,0.,0.));
#9151=DIRECTION('center_axis',(0.,0.,1.));
#9152=DIRECTION('ref_axis',(1.,0.,0.));
#9153=DIRECTION('',(0.,0.,1.));
#9154=DIRECTION('center_axis',(0.,0.,-1.));
#9155=DIRECTION('ref_axis',(1.,0.,0.));
#9156=DIRECTION('center_axis',(0.,0.,1.));
#9157=DIRECTION('ref_axis',(1.,0.,0.));
#9158=DIRECTION('center_axis',(0.,0.,1.));
#9159=DIRECTION('ref_axis',(1.,0.,0.));
#9160=DIRECTION('center_axis',(0.,0.,1.));
#9161=DIRECTION('ref_axis',(1.,0.,0.));
#9162=DIRECTION('center_axis',(0.,0.,1.));
#9163=DIRECTION('ref_axis',(1.,0.,0.));
#9164=DIRECTION('',(0.,0.,1.));
#9165=DIRECTION('center_axis',(0.,0.,-1.));
#9166=DIRECTION('ref_axis',(1.,0.,0.));
#9167=DIRECTION('center_axis',(0.,0.,1.));
#9168=DIRECTION('ref_axis',(1.,0.,0.));
#9169=DIRECTION('center_axis',(0.,0.,1.));
#9170=DIRECTION('ref_axis',(1.,0.,0.));
#9171=DIRECTION('center_axis',(0.,0.,1.));
#9172=DIRECTION('ref_axis',(1.,0.,0.));
#9173=DIRECTION('center_axis',(0.,0.,1.));
#9174=DIRECTION('ref_axis',(1.,0.,0.));
#9175=DIRECTION('',(0.,0.,1.));
#9176=DIRECTION('center_axis',(0.,0.,1.));
#9177=DIRECTION('ref_axis',(1.,0.,0.));
#9178=DIRECTION('center_axis',(0.,0.,1.));
#9179=DIRECTION('ref_axis',(1.,0.,0.));
#9180=DIRECTION('',(0.,0.,1.));
#9181=DIRECTION('center_axis',(0.,0.,1.));
#9182=DIRECTION('ref_axis',(1.,0.,0.));
#9183=DIRECTION('center_axis',(0.,0.,1.));
#9184=DIRECTION('ref_axis',(1.,0.,0.));
#9185=DIRECTION('',(0.,0.,1.));
#9186=DIRECTION('center_axis',(0.,0.,1.));
#9187=DIRECTION('ref_axis',(1.,0.,0.));
#9188=DIRECTION('center_axis',(0.,0.,1.));
#9189=DIRECTION('ref_axis',(1.,0.,0.));
#9190=DIRECTION('',(0.,0.,1.));
#9191=DIRECTION('center_axis',(0.,-0.56333682464151,0.826227342807548));
#9192=DIRECTION('ref_axis',(0.,-0.826227342807548,-0.56333682464151));
#9193=DIRECTION('',(0.,-0.826227342807548,-0.56333682464151));
#9194=DIRECTION('',(1.,0.,0.));
#9195=DIRECTION('',(0.,-0.826227342807548,-0.56333682464151));
#9196=DIRECTION('',(1.,0.,0.));
#9197=DIRECTION('center_axis',(0.,-1.,0.));
#9198=DIRECTION('ref_axis',(0.,0.,-1.));
#9199=DIRECTION('',(0.,0.,-1.));
#9200=DIRECTION('',(0.,0.,-1.));
#9201=DIRECTION('',(1.,0.,0.));
#9202=DIRECTION('center_axis',(0.,-0.56333682464151,-0.826227342807548));
#9203=DIRECTION('ref_axis',(0.,0.826227342807548,-0.56333682464151));
#9204=DIRECTION('',(0.,0.826227342807548,-0.56333682464151));
#9205=DIRECTION('',(0.,0.826227342807548,-0.56333682464151));
#9206=DIRECTION('',(1.,0.,0.));
#9207=DIRECTION('center_axis',(0.,-1.,0.));
#9208=DIRECTION('ref_axis',(0.,0.,-1.));
#9209=DIRECTION('',(0.,0.,-1.));
#9210=DIRECTION('',(0.,0.,-1.));
#9211=DIRECTION('',(1.,0.,0.));
#9212=DIRECTION('center_axis',(0.,0.,1.));
#9213=DIRECTION('ref_axis',(0.,-1.,0.));
#9214=DIRECTION('',(0.,-1.,0.));
#9215=DIRECTION('',(0.,-1.,0.));
#9216=DIRECTION('',(1.,0.,0.));
#9217=DIRECTION('center_axis',(0.,1.,0.));
#9218=DIRECTION('ref_axis',(0.,0.,1.));
#9219=DIRECTION('',(0.,0.,1.));
#9220=DIRECTION('',(0.,0.,1.));
#9221=DIRECTION('',(1.,0.,0.));
#9222=DIRECTION('center_axis',(0.,0.56333682464151,-0.826227342807548));
#9223=DIRECTION('ref_axis',(0.,0.826227342807548,0.56333682464151));
#9224=DIRECTION('',(0.,0.826227342807548,0.56333682464151));
#9225=DIRECTION('',(0.,0.826227342807548,0.56333682464151));
#9226=DIRECTION('',(1.,0.,0.));
#9227=DIRECTION('center_axis',(0.,1.,0.));
#9228=DIRECTION('ref_axis',(0.,0.,1.));
#9229=DIRECTION('',(0.,0.,1.));
#9230=DIRECTION('',(0.,0.,1.));
#9231=DIRECTION('',(1.,0.,0.));
#9232=DIRECTION('center_axis',(0.,0.56333682464151,0.826227342807548));
#9233=DIRECTION('ref_axis',(0.,-0.826227342807548,0.56333682464151));
#9234=DIRECTION('',(0.,-0.826227342807548,0.56333682464151));
#9235=DIRECTION('',(0.,-0.826227342807548,0.56333682464151));
#9236=DIRECTION('',(1.,0.,0.));
#9237=DIRECTION('center_axis',(0.,1.,0.));
#9238=DIRECTION('ref_axis',(0.,0.,1.));
#9239=DIRECTION('',(0.,0.,1.));
#9240=DIRECTION('',(0.,0.,1.));
#9241=DIRECTION('',(1.,0.,0.));
#9242=DIRECTION('center_axis',(0.,0.,-1.));
#9243=DIRECTION('ref_axis',(0.,1.,0.));
#9244=DIRECTION('',(0.,1.,0.));
#9245=DIRECTION('',(0.,1.,0.));
#9246=DIRECTION('',(1.,0.,0.));
#9247=DIRECTION('center_axis',(0.,-1.,0.));
#9248=DIRECTION('ref_axis',(0.,0.,-1.));
#9249=DIRECTION('',(0.,0.,-1.));
#9250=DIRECTION('',(0.,0.,-1.));
#9251=DIRECTION('center_axis',(1.,0.,0.));
#9252=DIRECTION('ref_axis',(0.,0.,-1.));
#9253=DIRECTION('center_axis',(1.,0.,0.));
#9254=DIRECTION('ref_axis',(0.,0.,-1.));
#9255=DIRECTION('axis',(0.,0.,1.));
#9256=DIRECTION('refdir',(1.,0.,0.));
#9257=DIRECTION('center_axis',(0.866025403784439,0.,-0.5));
#9258=DIRECTION('ref_axis',(0.5,0.,0.866025403784439));
#9259=DIRECTION('',(-0.5,0.,-0.866025403784439));
#9260=DIRECTION('',(0.,-1.,0.));
#9261=DIRECTION('',(0.5,0.,0.866025403784439));
#9262=DIRECTION('',(0.,-1.,0.));
#9263=DIRECTION('center_axis',(1.20185167898973E-16,0.,-1.));
#9264=DIRECTION('ref_axis',(1.,0.,1.20185167898973E-16));
#9265=DIRECTION('',(-1.,0.,-1.20185167898973E-16));
#9266=DIRECTION('',(0.,-1.,0.));
#9267=DIRECTION('',(1.,0.,1.20185167898973E-16));
#9268=DIRECTION('center_axis',(-0.866025403784439,0.,-0.5));
#9269=DIRECTION('ref_axis',(0.5,0.,-0.866025403784439));
#9270=DIRECTION('',(-0.5,0.,0.866025403784439));
#9271=DIRECTION('',(0.,-1.,0.));
#9272=DIRECTION('',(0.5,0.,-0.866025403784439));
#9273=DIRECTION('center_axis',(-0.866025403784439,0.,0.5));
#9274=DIRECTION('ref_axis',(-0.5,0.,-0.866025403784439));
#9275=DIRECTION('',(0.5,0.,0.866025403784439));
#9276=DIRECTION('',(0.,-1.,0.));
#9277=DIRECTION('',(-0.5,0.,-0.866025403784439));
#9278=DIRECTION('center_axis',(-2.40370335797945E-16,0.,1.));
#9279=DIRECTION('ref_axis',(-1.,0.,-2.40370335797945E-16));
#9280=DIRECTION('',(1.,0.,2.40370335797945E-16));
#9281=DIRECTION('',(0.,-1.,0.));
#9282=DIRECTION('',(-1.,0.,-2.40370335797945E-16));
#9283=DIRECTION('center_axis',(0.866025403784439,0.,0.5));
#9284=DIRECTION('ref_axis',(-0.5,0.,0.866025403784439));
#9285=DIRECTION('',(0.5,0.,-0.866025403784439));
#9286=DIRECTION('',(-0.5,0.,0.866025403784439));
#9287=DIRECTION('center_axis',(0.,1.,0.));
#9288=DIRECTION('ref_axis',(1.,0.,0.));
#9289=DIRECTION('center_axis',(0.,-1.,0.));
#9290=DIRECTION('ref_axis',(0.,0.,-1.));
#9291=DIRECTION('center_axis',(0.,1.,0.));
#9292=DIRECTION('ref_axis',(1.,0.,0.));
#9293=DIRECTION('center_axis',(0.,1.,0.));
#9294=DIRECTION('ref_axis',(1.,0.,0.));
#9295=DIRECTION('center_axis',(0.,1.,0.));
#9296=DIRECTION('ref_axis',(1.,0.,0.));
#9297=DIRECTION('center_axis',(0.,1.,0.));
#9298=DIRECTION('ref_axis',(1.,0.,0.));
#9299=DIRECTION('',(0.,-1.,0.));
#9300=DIRECTION('center_axis',(0.,1.,0.));
#9301=DIRECTION('ref_axis',(1.,0.,0.));
#9302=DIRECTION('center_axis',(0.,1.,0.));
#9303=DIRECTION('ref_axis',(1.,0.,0.));
#9304=DIRECTION('center_axis',(0.,1.,0.));
#9305=DIRECTION('ref_axis',(0.,0.,1.));
#9306=DIRECTION('center_axis',(0.,-1.,0.));
#9307=DIRECTION('ref_axis',(1.,0.,0.));
#9308=DIRECTION('center_axis',(0.,-1.,0.));
#9309=DIRECTION('ref_axis',(1.,0.,0.));
#9310=DIRECTION('center_axis',(0.,-1.,0.));
#9311=DIRECTION('ref_axis',(1.,0.,0.));
#9312=DIRECTION('',(0.707106781186548,0.707106781186547,8.65956056235493E-17));
#9313=DIRECTION('center_axis',(0.,-1.,0.));
#9314=DIRECTION('ref_axis',(1.,0.,0.));
#9315=DIRECTION('center_axis',(0.,-1.,0.));
#9316=DIRECTION('ref_axis',(1.,0.,0.));
#9317=DIRECTION('',(0.,1.,0.));
#9318=DIRECTION('center_axis',(0.,1.,0.));
#9319=DIRECTION('ref_axis',(1.,0.,0.));
#9320=DIRECTION('center_axis',(0.,-1.,0.));
#9321=DIRECTION('ref_axis',(1.,0.,0.));
#9322=DIRECTION('',(-0.707106781186547,0.707106781186548,-8.65956056235493E-17));
#9323=DIRECTION('center_axis',(0.,-1.,0.));
#9324=DIRECTION('ref_axis',(0.,0.,-1.));
#9325=DIRECTION('center_axis',(0.,-1.,0.));
#9326=DIRECTION('ref_axis',(1.,0.,0.));
#9327=DIRECTION('center_axis',(0.,1.,0.));
#9328=DIRECTION('ref_axis',(1.,0.,0.));
#9329=DIRECTION('center_axis',(0.,1.,0.));
#9330=DIRECTION('ref_axis',(1.,0.,0.));
#9331=DIRECTION('',(-0.447213595499958,0.894427190999916,-5.47678698264203E-17));
#9332=DIRECTION('center_axis',(0.,-1.,0.));
#9333=DIRECTION('ref_axis',(1.,0.,0.));
#9334=DIRECTION('',(0.,1.,0.));
#9335=DIRECTION('axis',(0.,0.,1.));
#9336=DIRECTION('refdir',(1.,0.,0.));
#9337=DIRECTION('center_axis',(0.,1.,0.));
#9338=DIRECTION('ref_axis',(0.,0.,1.));
#9339=DIRECTION('center_axis',(0.,-1.,0.));
#9340=DIRECTION('ref_axis',(1.,0.,0.));
#9341=DIRECTION('center_axis',(0.,-1.,0.));
#9342=DIRECTION('ref_axis',(1.,0.,0.));
#9343=DIRECTION('center_axis',(0.,-1.,0.));
#9344=DIRECTION('ref_axis',(1.,0.,0.));
#9345=DIRECTION('',(0.707106781186548,0.707106781186547,8.65956056235493E-17));
#9346=DIRECTION('center_axis',(0.,-1.,0.));
#9347=DIRECTION('ref_axis',(1.,0.,0.));
#9348=DIRECTION('center_axis',(0.,-1.,0.));
#9349=DIRECTION('ref_axis',(1.,0.,0.));
#9350=DIRECTION('',(0.,1.,0.));
#9351=DIRECTION('center_axis',(0.,1.,0.));
#9352=DIRECTION('ref_axis',(1.,0.,0.));
#9353=DIRECTION('center_axis',(0.,-1.,0.));
#9354=DIRECTION('ref_axis',(1.,0.,0.));
#9355=DIRECTION('',(-0.707106781186547,0.707106781186548,-8.65956056235493E-17));
#9356=DIRECTION('center_axis',(0.,-1.,0.));
#9357=DIRECTION('ref_axis',(0.,0.,-1.));
#9358=DIRECTION('center_axis',(0.,-1.,0.));
#9359=DIRECTION('ref_axis',(1.,0.,0.));
#9360=DIRECTION('center_axis',(0.,1.,0.));
#9361=DIRECTION('ref_axis',(1.,0.,0.));
#9362=DIRECTION('center_axis',(0.,1.,0.));
#9363=DIRECTION('ref_axis',(1.,0.,0.));
#9364=DIRECTION('',(-0.447213595499958,0.894427190999916,-5.47678698264203E-17));
#9365=DIRECTION('center_axis',(0.,-1.,0.));
#9366=DIRECTION('ref_axis',(1.,0.,0.));
#9367=DIRECTION('center_axis',(0.,1.,0.));
#9368=DIRECTION('ref_axis',(1.,0.,0.));
#9369=DIRECTION('',(0.,1.,0.));
#9370=DIRECTION('center_axis',(0.,1.,0.));
#9371=DIRECTION('ref_axis',(1.,0.,0.));
#9372=DIRECTION('center_axis',(0.,-1.,0.));
#9373=DIRECTION('ref_axis',(1.,0.,0.));
#9374=DIRECTION('',(-0.707106781186547,0.707106781186548,-8.65956056235493E-17));
#9375=DIRECTION('center_axis',(0.,-1.,0.));
#9376=DIRECTION('ref_axis',(0.,0.,-1.));
#9377=DIRECTION('center_axis',(0.866025403784439,0.,-0.5));
#9378=DIRECTION('ref_axis',(0.5,0.,0.866025403784439));
#9379=DIRECTION('',(-0.5,0.,-0.866025403784439));
#9380=DIRECTION('',(0.,-1.,0.));
#9381=DIRECTION('',(0.5,0.,0.866025403784439));
#9382=DIRECTION('',(0.,-1.,0.));
#9383=DIRECTION('center_axis',(1.20185167898973E-16,0.,-1.));
#9384=DIRECTION('ref_axis',(1.,0.,1.20185167898973E-16));
#9385=DIRECTION('',(-1.,0.,-1.20185167898973E-16));
#9386=DIRECTION('',(0.,-1.,0.));
#9387=DIRECTION('',(1.,0.,1.20185167898973E-16));
#9388=DIRECTION('center_axis',(-0.866025403784439,0.,-0.5));
#9389=DIRECTION('ref_axis',(0.5,0.,-0.866025403784439));
#9390=DIRECTION('',(-0.5,0.,0.866025403784439));
#9391=DIRECTION('',(0.,-1.,0.));
#9392=DIRECTION('',(0.5,0.,-0.866025403784439));
#9393=DIRECTION('center_axis',(-0.866025403784439,0.,0.5));
#9394=DIRECTION('ref_axis',(-0.5,0.,-0.866025403784439));
#9395=DIRECTION('',(0.5,0.,0.866025403784439));
#9396=DIRECTION('',(0.,-1.,0.));
#9397=DIRECTION('',(-0.5,0.,-0.866025403784439));
#9398=DIRECTION('center_axis',(-2.40370335797945E-16,0.,1.));
#9399=DIRECTION('ref_axis',(-1.,0.,-2.40370335797945E-16));
#9400=DIRECTION('',(1.,0.,2.40370335797945E-16));
#9401=DIRECTION('',(0.,-1.,0.));
#9402=DIRECTION('',(-1.,0.,-2.40370335797945E-16));
#9403=DIRECTION('center_axis',(0.866025403784439,0.,0.5));
#9404=DIRECTION('ref_axis',(-0.5,0.,0.866025403784439));
#9405=DIRECTION('',(0.5,0.,-0.866025403784439));
#9406=DIRECTION('',(-0.5,0.,0.866025403784439));
#9407=DIRECTION('center_axis',(0.,1.,0.));
#9408=DIRECTION('ref_axis',(1.,0.,0.));
#9409=DIRECTION('center_axis',(0.,-1.,0.));
#9410=DIRECTION('ref_axis',(0.,0.,-1.));
#9411=DIRECTION('axis',(0.,0.,1.));
#9412=DIRECTION('refdir',(1.,0.,0.));
#9413=DIRECTION('center_axis',(0.,0.,1.));
#9414=DIRECTION('ref_axis',(1.,0.,0.));
#9415=DIRECTION('',(1.,0.,0.));
#9416=DIRECTION('',(0.,-1.,0.));
#9417=DIRECTION('',(-1.,0.,0.));
#9418=DIRECTION('',(0.,1.,0.));
#9419=DIRECTION('center_axis',(0.,1.,0.));
#9420=DIRECTION('ref_axis',(-1.,0.,0.));
#9421=DIRECTION('',(0.,0.,1.));
#9422=DIRECTION('',(-1.,0.,0.));
#9423=DIRECTION('',(0.,0.,1.));
#9424=DIRECTION('center_axis',(0.,0.,1.));
#9425=DIRECTION('ref_axis',(1.,0.,0.));
#9426=DIRECTION('',(0.,-1.,0.));
#9427=DIRECTION('',(1.,0.,0.));
#9428=DIRECTION('',(0.,1.,0.));
#9429=DIRECTION('center_axis',(0.,0.,-1.));
#9430=DIRECTION('ref_axis',(1.,0.,0.));
#9431=DIRECTION('center_axis',(-1.,0.,0.));
#9432=DIRECTION('ref_axis',(0.,-1.,0.));
#9433=DIRECTION('',(0.,0.,1.));
#9434=DIRECTION('',(0.,0.707106781186548,0.707106781186548));
#9435=DIRECTION('',(0.,-1.,0.));
#9436=DIRECTION('',(0.,0.707106781186548,-0.707106781186548));
#9437=DIRECTION('',(0.,0.,1.));
#9438=DIRECTION('',(0.,-1.,0.));
#9439=DIRECTION('',(0.,0.,1.));
#9440=DIRECTION('center_axis',(0.,-1.,0.));
#9441=DIRECTION('ref_axis',(1.,0.,0.));
#9442=DIRECTION('',(1.,0.,0.));
#9443=DIRECTION('',(0.,0.,1.));
#9444=DIRECTION('center_axis',(0.,0.,1.));
#9445=DIRECTION('ref_axis',(1.,0.,0.));
#9446=DIRECTION('',(-1.,0.,0.));
#9447=DIRECTION('',(0.,1.,0.));
#9448=DIRECTION('center_axis',(1.,0.,0.));
#9449=DIRECTION('ref_axis',(0.,1.,0.));
#9450=DIRECTION('',(0.,0.,1.));
#9451=DIRECTION('',(0.,-0.707106781186548,0.707106781186548));
#9452=DIRECTION('',(0.,1.,0.));
#9453=DIRECTION('',(0.,-0.707106781186548,-0.707106781186548));
#9454=DIRECTION('',(0.,0.,1.));
#9455=DIRECTION('center_axis',(0.,-1.,0.));
#9456=DIRECTION('ref_axis',(1.,0.,0.));
#9457=DIRECTION('',(-1.,0.,0.));
#9458=DIRECTION('center_axis',(0.,-0.707106781186548,-0.707106781186548));
#9459=DIRECTION('ref_axis',(-1.,0.,0.));
#9460=DIRECTION('',(1.,0.,0.));
#9461=DIRECTION('center_axis',(0.,0.707106781186548,0.707106781186548));
#9462=DIRECTION('ref_axis',(0.,0.707106781186547,-0.707106781186547));
#9463=DIRECTION('',(1.,0.,0.));
#9464=DIRECTION('center_axis',(0.,0.,1.));
#9465=DIRECTION('ref_axis',(1.,0.,0.));
#9466=DIRECTION('center_axis',(0.,0.,-1.));
#9467=DIRECTION('ref_axis',(1.,0.,0.));
#9468=DIRECTION('',(0.,0.,1.));
#9469=DIRECTION('center_axis',(0.,0.,-1.));
#9470=DIRECTION('ref_axis',(1.,0.,0.));
#9471=DIRECTION('center_axis',(0.,-0.707106781186548,0.707106781186548));
#9472=DIRECTION('ref_axis',(0.,0.707106781186547,0.707106781186547));
#9473=DIRECTION('center_axis',(0.,0.,-1.));
#9474=DIRECTION('ref_axis',(1.,0.,0.));
#9475=DIRECTION('center_axis',(0.,0.,1.));
#9476=DIRECTION('ref_axis',(1.,0.,0.));
#9477=DIRECTION('',(-1.,0.,0.));
#9478=DIRECTION('center_axis',(0.,0.,1.));
#9479=DIRECTION('ref_axis',(1.,0.,0.));
#9480=DIRECTION('',(-1.,0.,0.));
#9481=DIRECTION('center_axis',(0.,0.707106781186548,-0.707106781186548));
#9482=DIRECTION('ref_axis',(-1.,0.,0.));
#9483=DIRECTION('',(1.,0.,0.));
#9484=DIRECTION('center_axis',(0.,1.,0.));
#9485=DIRECTION('ref_axis',(-1.,0.,0.));
#9486=DIRECTION('axis',(0.,0.,1.));
#9487=DIRECTION('refdir',(1.,0.,0.));
#9488=DIRECTION('center_axis',(0.,1.,0.));
#9489=DIRECTION('ref_axis',(1.,0.,0.));
#9490=DIRECTION('center_axis',(0.,1.,0.));
#9491=DIRECTION('ref_axis',(1.,0.,0.));
#9492=DIRECTION('',(0.707106781186548,-0.707106781186547,-8.65956056235494E-17));
#9493=DIRECTION('center_axis',(0.,-1.,0.));
#9494=DIRECTION('ref_axis',(1.,0.,0.));
#9495=DIRECTION('center_axis',(0.,1.,0.));
#9496=DIRECTION('ref_axis',(1.,0.,0.));
#9497=DIRECTION('',(0.,-1.,0.));
#9498=DIRECTION('center_axis',(0.,-1.,0.));
#9499=DIRECTION('ref_axis',(1.,0.,0.));
#9500=DIRECTION('center_axis',(0.,1.,0.));
#9501=DIRECTION('ref_axis',(1.,0.,0.));
#9502=DIRECTION('center_axis',(0.,1.,0.));
#9503=DIRECTION('ref_axis',(1.,0.,0.));
#9504=DIRECTION('center_axis',(0.,1.,0.));
#9505=DIRECTION('ref_axis',(1.,0.,0.));
#9506=DIRECTION('',(0.,-1.,0.));
#9507=DIRECTION('center_axis',(0.,1.,0.));
#9508=DIRECTION('ref_axis',(1.,0.,0.));
#9509=DIRECTION('center_axis',(0.,1.,0.));
#9510=DIRECTION('ref_axis',(1.,0.,0.));
#9511=DIRECTION('axis',(0.,0.,1.));
#9512=DIRECTION('refdir',(1.,0.,0.));
#9513=DIRECTION('axis',(0.,0.,1.));
#9514=DIRECTION('refdir',(1.,0.,0.));
#9515=DIRECTION('center_axis',(1.,0.,0.));
#9516=DIRECTION('ref_axis',(0.,0.,-1.));
#9517=DIRECTION('center_axis',(1.,0.,0.));
#9518=DIRECTION('ref_axis',(0.,0.,-1.));
#9519=DIRECTION('',(1.,0.,0.));
#9520=DIRECTION('center_axis',(-1.,0.,0.));
#9521=DIRECTION('ref_axis',(0.,0.,-1.));
#9522=DIRECTION('center_axis',(0.,0.,1.));
#9523=DIRECTION('ref_axis',(1.,0.,0.));
#9524=DIRECTION('',(1.,0.,0.));
#9525=DIRECTION('',(0.,-1.,0.));
#9526=DIRECTION('',(-1.,0.,0.));
#9527=DIRECTION('',(0.,1.,0.));
#9528=DIRECTION('center_axis',(0.,1.,0.));
#9529=DIRECTION('ref_axis',(-1.,0.,0.));
#9530=DIRECTION('',(0.,0.,1.));
#9531=DIRECTION('',(-1.,0.,0.));
#9532=DIRECTION('',(0.,0.,1.));
#9533=DIRECTION('center_axis',(0.,0.,1.));
#9534=DIRECTION('ref_axis',(1.,0.,0.));
#9535=DIRECTION('',(-1.,0.,0.));
#9536=DIRECTION('',(0.,1.,0.));
#9537=DIRECTION('',(0.,-1.,0.));
#9538=DIRECTION('center_axis',(0.,1.,0.));
#9539=DIRECTION('ref_axis',(-1.,0.,0.));
#9540=DIRECTION('',(0.,0.,1.));
#9541=DIRECTION('',(-1.,0.,0.));
#9542=DIRECTION('',(0.,0.,1.));
#9543=DIRECTION('center_axis',(0.,1.,0.));
#9544=DIRECTION('ref_axis',(-1.,0.,0.));
#9545=DIRECTION('',(0.,0.,1.));
#9546=DIRECTION('',(0.,0.,1.));
#9547=DIRECTION('',(0.,0.,1.));
#9548=DIRECTION('',(-1.,0.,0.));
#9549=DIRECTION('',(0.,0.,1.));
#9550=DIRECTION('center_axis',(0.,0.,1.));
#9551=DIRECTION('ref_axis',(1.,0.,0.));
#9552=DIRECTION('center_axis',(0.,0.,1.));
#9553=DIRECTION('ref_axis',(1.,0.,0.));
#9554=DIRECTION('',(0.,0.,1.));
#9555=DIRECTION('center_axis',(0.,0.,-1.));
#9556=DIRECTION('ref_axis',(1.,0.,0.));
#9557=DIRECTION('center_axis',(0.,0.,1.));
#9558=DIRECTION('ref_axis',(1.,0.,0.));
#9559=DIRECTION('center_axis',(0.,0.,1.));
#9560=DIRECTION('ref_axis',(1.,0.,0.));
#9561=DIRECTION('',(0.,0.,1.));
#9562=DIRECTION('center_axis',(0.,0.,-1.));
#9563=DIRECTION('ref_axis',(1.,0.,0.));
#9564=DIRECTION('center_axis',(0.,0.,1.));
#9565=DIRECTION('ref_axis',(1.,0.,0.));
#9566=DIRECTION('center_axis',(0.,0.,1.));
#9567=DIRECTION('ref_axis',(1.,0.,0.));
#9568=DIRECTION('',(0.,0.,1.));
#9569=DIRECTION('center_axis',(0.,0.,-1.));
#9570=DIRECTION('ref_axis',(1.,0.,0.));
#9571=DIRECTION('center_axis',(1.,0.,0.));
#9572=DIRECTION('ref_axis',(0.,-1.22464679914735E-16,1.));
#9573=DIRECTION('',(1.,0.,0.));
#9574=DIRECTION('center_axis',(1.,0.,0.));
#9575=DIRECTION('ref_axis',(0.,0.,-1.));
#9576=DIRECTION('',(-1.,0.,0.));
#9577=DIRECTION('center_axis',(1.,0.,0.));
#9578=DIRECTION('ref_axis',(0.,0.,-1.));
#9579=DIRECTION('center_axis',(1.,0.,0.));
#9580=DIRECTION('ref_axis',(0.,0.,-1.));
#9581=DIRECTION('',(0.,-1.,0.));
#9582=DIRECTION('center_axis',(-1.,0.,0.));
#9583=DIRECTION('ref_axis',(0.,-1.,0.));
#9584=DIRECTION('',(0.,-1.,0.));
#9585=DIRECTION('',(0.,0.,1.));
#9586=DIRECTION('',(0.,1.,0.));
#9587=DIRECTION('center_axis',(1.,0.,0.));
#9588=DIRECTION('ref_axis',(0.,0.,-1.));
#9589=DIRECTION('',(0.,1.,0.));
#9590=DIRECTION('',(0.,1.,0.));
#9591=DIRECTION('center_axis',(1.,0.,0.));
#9592=DIRECTION('ref_axis',(0.,0.,-1.));
#9593=DIRECTION('center_axis',(1.,0.,0.));
#9594=DIRECTION('ref_axis',(0.,0.,-1.));
#9595=DIRECTION('center_axis',(-1.,0.,0.));
#9596=DIRECTION('ref_axis',(0.,0.,-1.));
#9597=DIRECTION('center_axis',(1.,0.,0.));
#9598=DIRECTION('ref_axis',(0.,0.,-1.));
#9599=DIRECTION('center_axis',(1.,0.,0.));
#9600=DIRECTION('ref_axis',(0.,0.,-1.));
#9601=DIRECTION('',(1.,0.,0.));
#9602=DIRECTION('center_axis',(-1.,0.,0.));
#9603=DIRECTION('ref_axis',(0.,0.,-1.));
#9604=DIRECTION('center_axis',(0.,0.,1.));
#9605=DIRECTION('ref_axis',(1.,0.,0.));
#9606=DIRECTION('',(-1.,0.,0.));
#9607=DIRECTION('',(0.,-1.,0.));
#9608=DIRECTION('',(1.,0.,0.));
#9609=DIRECTION('',(0.,1.,0.));
#9610=DIRECTION('',(1.,0.,0.));
#9611=DIRECTION('',(0.,-1.,0.));
#9612=DIRECTION('',(-1.,0.,0.));
#9613=DIRECTION('',(0.,1.,0.));
#9614=DIRECTION('center_axis',(1.,0.,0.));
#9615=DIRECTION('ref_axis',(0.,0.,-1.));
#9616=DIRECTION('',(1.,0.,0.));
#9617=DIRECTION('center_axis',(-1.,0.,0.));
#9618=DIRECTION('ref_axis',(0.,0.,-1.));
#9619=DIRECTION('center_axis',(1.,0.,0.));
#9620=DIRECTION('ref_axis',(0.,-1.22464679914735E-16,1.));
#9621=DIRECTION('center_axis',(1.,0.,0.));
#9622=DIRECTION('ref_axis',(0.,0.,-1.));
#9623=DIRECTION('center_axis',(1.,0.,0.));
#9624=DIRECTION('ref_axis',(0.,0.,-1.));
#9625=DIRECTION('center_axis',(1.,0.,0.));
#9626=DIRECTION('ref_axis',(0.,0.,-1.));
#9627=DIRECTION('',(1.,0.,0.));
#9628=DIRECTION('center_axis',(-1.,0.,0.));
#9629=DIRECTION('ref_axis',(0.,0.,-1.));
#9630=DIRECTION('center_axis',(1.,0.,0.));
#9631=DIRECTION('ref_axis',(0.,0.,-1.));
#9632=DIRECTION('',(1.,0.,0.));
#9633=DIRECTION('center_axis',(-1.,0.,0.));
#9634=DIRECTION('ref_axis',(0.,0.,-1.));
#9635=DIRECTION('center_axis',(1.,0.,0.));
#9636=DIRECTION('ref_axis',(0.,1.,0.));
#9637=DIRECTION('',(0.,0.,1.));
#9638=DIRECTION('',(0.,1.,0.));
#9639=DIRECTION('',(0.,0.,1.));
#9640=DIRECTION('center_axis',(1.,0.,0.));
#9641=DIRECTION('ref_axis',(0.,1.,0.));
#9642=DIRECTION('',(0.,0.,1.));
#9643=DIRECTION('',(0.,1.,0.));
#9644=DIRECTION('center_axis',(0.,1.,0.));
#9645=DIRECTION('ref_axis',(-1.,0.,0.));
#9646=DIRECTION('',(0.,0.,1.));
#9647=DIRECTION('',(-1.,0.,0.));
#9648=DIRECTION('center_axis',(0.,-1.,0.));
#9649=DIRECTION('ref_axis',(1.,0.,0.));
#9650=DIRECTION('',(1.,0.,0.));
#9651=DIRECTION('',(0.,0.,1.));
#9652=DIRECTION('center_axis',(-1.,0.,0.));
#9653=DIRECTION('ref_axis',(0.,-1.,0.));
#9654=DIRECTION('',(0.,-1.,0.));
#9655=DIRECTION('center_axis',(0.,0.,1.));
#9656=DIRECTION('ref_axis',(1.,0.,0.));
#9657=DIRECTION('',(0.,-1.,0.));
#9658=DIRECTION('center_axis',(-1.,0.,0.));
#9659=DIRECTION('ref_axis',(0.,-1.,0.));
#9660=DIRECTION('',(0.,0.,1.));
#9661=DIRECTION('',(0.,-1.,0.));
#9662=DIRECTION('center_axis',(1.,0.,0.));
#9663=DIRECTION('ref_axis',(0.,1.,0.));
#9664=DIRECTION('',(0.,1.,0.));
#9665=DIRECTION('',(0.,0.,1.));
#9666=DIRECTION('',(0.,1.,0.));
#9667=DIRECTION('center_axis',(0.,-1.,0.));
#9668=DIRECTION('ref_axis',(1.,0.,0.));
#9669=DIRECTION('',(1.,0.,0.));
#9670=DIRECTION('',(1.,0.,0.));
#9671=DIRECTION('center_axis',(0.,0.,1.));
#9672=DIRECTION('ref_axis',(1.,0.,0.));
#9673=DIRECTION('center_axis',(0.,0.,1.));
#9674=DIRECTION('ref_axis',(1.,0.,0.));
#9675=DIRECTION('axis',(0.,0.,1.));
#9676=DIRECTION('refdir',(1.,0.,0.));
#9677=DIRECTION('center_axis',(0.,0.,1.));
#9678=DIRECTION('ref_axis',(1.,0.,0.));
#9679=DIRECTION('center_axis',(0.,0.,1.));
#9680=DIRECTION('ref_axis',(1.,0.,0.));
#9681=DIRECTION('',(0.,0.,1.));
#9682=DIRECTION('center_axis',(0.,0.,-1.));
#9683=DIRECTION('ref_axis',(1.,0.,0.));
#9684=DIRECTION('center_axis',(0.,0.,1.));
#9685=DIRECTION('ref_axis',(1.,0.,0.));
#9686=DIRECTION('center_axis',(0.,0.,1.));
#9687=DIRECTION('ref_axis',(1.,0.,0.));
#9688=DIRECTION('',(0.,0.,-1.));
#9689=DIRECTION('center_axis',(0.,0.,1.));
#9690=DIRECTION('ref_axis',(1.,0.,0.));
#9691=DIRECTION('center_axis',(0.,0.,1.));
#9692=DIRECTION('ref_axis',(1.,0.,0.));
#9693=DIRECTION('center_axis',(0.,0.,1.));
#9694=DIRECTION('ref_axis',(1.,0.,0.));
#9695=DIRECTION('axis',(0.,0.,1.));
#9696=DIRECTION('refdir',(1.,0.,0.));
#9697=DIRECTION('center_axis',(0.,0.,1.));
#9698=DIRECTION('ref_axis',(1.,0.,0.));
#9699=DIRECTION('center_axis',(0.,0.,1.));
#9700=DIRECTION('ref_axis',(1.,0.,0.));
#9701=DIRECTION('',(0.,0.,-1.));
#9702=DIRECTION('center_axis',(0.,0.,-1.));
#9703=DIRECTION('ref_axis',(1.,0.,0.));
#9704=DIRECTION('center_axis',(0.,0.,1.));
#9705=DIRECTION('ref_axis',(1.,0.,0.));
#9706=DIRECTION('center_axis',(0.,0.,1.));
#9707=DIRECTION('ref_axis',(1.,0.,0.));
#9708=DIRECTION('center_axis',(0.,0.,1.));
#9709=DIRECTION('ref_axis',(1.,0.,0.));
#9710=DIRECTION('',(0.,0.,-1.));
#9711=DIRECTION('center_axis',(0.,0.,1.));
#9712=DIRECTION('ref_axis',(1.,0.,0.));
#9713=DIRECTION('center_axis',(0.,0.,1.));
#9714=DIRECTION('ref_axis',(1.,0.,0.));
#9715=DIRECTION('center_axis',(0.,0.,1.));
#9716=DIRECTION('ref_axis',(1.,0.,0.));
#9717=DIRECTION('center_axis',(0.,0.,1.));
#9718=DIRECTION('ref_axis',(1.,0.,0.));
#9719=DIRECTION('center_axis',(0.,0.,1.));
#9720=DIRECTION('ref_axis',(1.,0.,0.));
#9721=DIRECTION('center_axis',(0.,0.,1.));
#9722=DIRECTION('ref_axis',(1.,0.,0.));
#9723=DIRECTION('center_axis',(0.,0.,1.));
#9724=DIRECTION('ref_axis',(1.,0.,0.));
#9725=DIRECTION('',(0.,0.,-1.));
#9726=DIRECTION('center_axis',(0.,0.,1.));
#9727=DIRECTION('ref_axis',(1.,0.,0.));
#9728=DIRECTION('center_axis',(0.,0.,1.));
#9729=DIRECTION('ref_axis',(1.,0.,0.));
#9730=DIRECTION('',(0.,0.,-1.));
#9731=DIRECTION('center_axis',(0.,0.,1.));
#9732=DIRECTION('ref_axis',(1.,0.,0.));
#9733=DIRECTION('center_axis',(0.,0.,1.));
#9734=DIRECTION('ref_axis',(1.,0.,0.));
#9735=DIRECTION('axis',(0.,0.,1.));
#9736=DIRECTION('refdir',(1.,0.,0.));
#9737=DIRECTION('center_axis',(0.,0.,1.));
#9738=DIRECTION('ref_axis',(1.,0.,0.));
#9739=DIRECTION('center_axis',(0.,0.,-1.));
#9740=DIRECTION('ref_axis',(1.,0.,0.));
#9741=DIRECTION('',(0.,0.,-1.));
#9742=DIRECTION('center_axis',(0.,0.,-1.));
#9743=DIRECTION('ref_axis',(1.,0.,0.));
#9744=DIRECTION('center_axis',(0.,0.,1.));
#9745=DIRECTION('ref_axis',(1.,0.,0.));
#9746=DIRECTION('center_axis',(0.,0.,1.));
#9747=DIRECTION('ref_axis',(1.,0.,0.));
#9748=DIRECTION('',(0.,0.,-1.));
#9749=DIRECTION('center_axis',(0.,0.,1.));
#9750=DIRECTION('ref_axis',(1.,0.,0.));
#9751=DIRECTION('center_axis',(0.,0.,1.));
#9752=DIRECTION('ref_axis',(1.,0.,0.));
#9753=DIRECTION('center_axis',(0.,0.,1.));
#9754=DIRECTION('ref_axis',(1.,0.,0.));
#9755=DIRECTION('axis',(0.,0.,1.));
#9756=DIRECTION('refdir',(1.,0.,0.));
#9757=DIRECTION('center_axis',(0.,1.,0.));
#9758=DIRECTION('ref_axis',(1.,0.,0.));
#9759=DIRECTION('center_axis',(0.,1.,0.));
#9760=DIRECTION('ref_axis',(1.,0.,0.));
#9761=DIRECTION('',(0.,1.,0.));
#9762=DIRECTION('center_axis',(0.,-1.,0.));
#9763=DIRECTION('ref_axis',(1.,0.,0.));
#9764=DIRECTION('center_axis',(1.,0.,0.));
#9765=DIRECTION('ref_axis',(0.,0.,-1.));
#9766=DIRECTION('center_axis',(1.,0.,0.));
#9767=DIRECTION('ref_axis',(0.,0.,-1.));
#9768=DIRECTION('',(1.,0.,0.));
#9769=DIRECTION('center_axis',(1.,0.,0.));
#9770=DIRECTION('ref_axis',(0.,0.,-1.));
#9771=DIRECTION('center_axis',(1.,0.,0.));
#9772=DIRECTION('ref_axis',(0.,0.,-1.));
#9773=DIRECTION('center_axis',(0.,1.,0.));
#9774=DIRECTION('ref_axis',(-1.,0.,0.));
#9775=DIRECTION('',(-1.,0.,0.));
#9776=DIRECTION('',(0.,0.,1.));
#9777=DIRECTION('',(-1.,0.,0.));
#9778=DIRECTION('',(0.,0.,1.));
#9779=DIRECTION('center_axis',(1.,0.,0.));
#9780=DIRECTION('ref_axis',(0.,1.,0.));
#9781=DIRECTION('',(0.,1.,0.));
#9782=DIRECTION('',(0.,1.,0.));
#9783=DIRECTION('',(0.,0.,1.));
#9784=DIRECTION('center_axis',(0.,-1.,0.));
#9785=DIRECTION('ref_axis',(1.,0.,0.));
#9786=DIRECTION('',(1.,0.,0.));
#9787=DIRECTION('',(1.,0.,0.));
#9788=DIRECTION('',(0.,0.,1.));
#9789=DIRECTION('center_axis',(-1.,0.,0.));
#9790=DIRECTION('ref_axis',(0.,-1.,0.));
#9791=DIRECTION('',(0.,-1.,0.));
#9792=DIRECTION('',(0.,-1.,0.));
#9793=DIRECTION('center_axis',(0.,0.,1.));
#9794=DIRECTION('ref_axis',(1.,0.,0.));
#9795=DIRECTION('center_axis',(0.,0.,1.));
#9796=DIRECTION('ref_axis',(1.,0.,0.));
#9797=DIRECTION('axis',(0.,0.,1.));
#9798=DIRECTION('refdir',(1.,0.,0.));
#9799=DIRECTION('center_axis',(0.,1.,0.));
#9800=DIRECTION('ref_axis',(-1.,0.,0.));
#9801=DIRECTION('',(-1.,0.,0.));
#9802=DIRECTION('',(0.,0.,1.));
#9803=DIRECTION('',(-1.,0.,0.));
#9804=DIRECTION('',(0.,0.,1.));
#9805=DIRECTION('center_axis',(1.,0.,0.));
#9806=DIRECTION('ref_axis',(0.,1.,0.));
#9807=DIRECTION('',(0.,1.,0.));
#9808=DIRECTION('',(0.,1.,0.));
#9809=DIRECTION('',(0.,0.,1.));
#9810=DIRECTION('center_axis',(0.,-1.,0.));
#9811=DIRECTION('ref_axis',(1.,0.,0.));
#9812=DIRECTION('',(1.,0.,0.));
#9813=DIRECTION('',(1.,0.,0.));
#9814=DIRECTION('',(0.,0.,1.));
#9815=DIRECTION('center_axis',(-1.,0.,0.));
#9816=DIRECTION('ref_axis',(0.,-1.,0.));
#9817=DIRECTION('',(0.,-1.,0.));
#9818=DIRECTION('',(0.,-1.,0.));
#9819=DIRECTION('center_axis',(0.,0.,1.));
#9820=DIRECTION('ref_axis',(1.,0.,0.));
#9821=DIRECTION('center_axis',(0.,0.,1.));
#9822=DIRECTION('ref_axis',(1.,0.,0.));
#9823=DIRECTION('axis',(0.,0.,1.));
#9824=DIRECTION('refdir',(1.,0.,0.));
#9825=DIRECTION('center_axis',(0.,1.,0.));
#9826=DIRECTION('ref_axis',(1.,0.,0.));
#9827=DIRECTION('center_axis',(0.,1.,0.));
#9828=DIRECTION('ref_axis',(1.,0.,0.));
#9829=DIRECTION('',(0.,-1.,0.));
#9830=DIRECTION('center_axis',(0.,1.,0.));
#9831=DIRECTION('ref_axis',(1.,0.,0.));
#9832=DIRECTION('center_axis',(0.,1.,0.));
#9833=DIRECTION('ref_axis',(1.,0.,0.));
#9834=DIRECTION('center_axis',(0.,1.,0.));
#9835=DIRECTION('ref_axis',(1.,0.,0.));
#9836=DIRECTION('center_axis',(0.,-1.,0.));
#9837=DIRECTION('ref_axis',(1.,0.,0.));
#9838=DIRECTION('center_axis',(0.,1.,0.));
#9839=DIRECTION('ref_axis',(1.,0.,0.));
#9840=DIRECTION('',(0.,-1.,0.));
#9841=DIRECTION('center_axis',(0.,1.,0.));
#9842=DIRECTION('ref_axis',(1.,0.,0.));
#9843=DIRECTION('center_axis',(0.,1.,0.));
#9844=DIRECTION('ref_axis',(1.,0.,0.));
#9845=DIRECTION('axis',(0.,0.,1.));
#9846=DIRECTION('refdir',(1.,0.,0.));
#9847=DIRECTION('axis',(0.,0.,1.));
#9848=DIRECTION('refdir',(1.,0.,0.));
#9849=DIRECTION('center_axis',(0.,0.,1.));
#9850=DIRECTION('ref_axis',(1.,0.,0.));
#9851=DIRECTION('',(-1.,0.,0.));
#9852=DIRECTION('center_axis',(0.,0.,1.));
#9853=DIRECTION('ref_axis',(1.,0.,0.));
#9854=DIRECTION('center_axis',(0.,0.,1.));
#9855=DIRECTION('ref_axis',(1.,0.,0.));
#9856=DIRECTION('',(0.,0.,-1.));
#9857=DIRECTION('center_axis',(0.,0.,1.));
#9858=DIRECTION('ref_axis',(1.,0.,0.));
#9859=DIRECTION('',(0.,0.,1.));
#9860=DIRECTION('center_axis',(0.,0.,-1.));
#9861=DIRECTION('ref_axis',(1.,0.,0.));
#9862=DIRECTION('center_axis',(0.,0.,1.));
#9863=DIRECTION('ref_axis',(1.,0.,0.));
#9864=DIRECTION('',(0.,0.,1.));
#9865=DIRECTION('center_axis',(0.,0.,1.));
#9866=DIRECTION('ref_axis',(1.,0.,0.));
#9867=DIRECTION('',(1.,0.,0.));
#9868=DIRECTION('center_axis',(0.,0.,1.));
#9869=DIRECTION('ref_axis',(1.,0.,0.));
#9870=DIRECTION('center_axis',(0.,0.,1.));
#9871=DIRECTION('ref_axis',(1.,0.,0.));
#9872=DIRECTION('',(0.,0.,-1.));
#9873=DIRECTION('center_axis',(0.,0.,1.));
#9874=DIRECTION('ref_axis',(1.,0.,0.));
#9875=DIRECTION('',(0.,0.,1.));
#9876=DIRECTION('center_axis',(0.,0.,-1.));
#9877=DIRECTION('ref_axis',(1.,0.,0.));
#9878=DIRECTION('center_axis',(0.,0.,1.));
#9879=DIRECTION('ref_axis',(1.,0.,0.));
#9880=DIRECTION('',(0.,0.,1.));
#9881=DIRECTION('center_axis',(0.,0.,1.));
#9882=DIRECTION('ref_axis',(1.,0.,0.));
#9883=DIRECTION('',(-1.,0.,0.));
#9884=DIRECTION('center_axis',(0.,0.,1.));
#9885=DIRECTION('ref_axis',(1.,0.,0.));
#9886=DIRECTION('center_axis',(0.,0.,1.));
#9887=DIRECTION('ref_axis',(1.,0.,0.));
#9888=DIRECTION('',(0.,0.,-1.));
#9889=DIRECTION('center_axis',(0.,0.,1.));
#9890=DIRECTION('ref_axis',(1.,0.,0.));
#9891=DIRECTION('',(0.,0.,1.));
#9892=DIRECTION('center_axis',(0.,0.,-1.));
#9893=DIRECTION('ref_axis',(1.,0.,0.));
#9894=DIRECTION('center_axis',(0.,0.,1.));
#9895=DIRECTION('ref_axis',(1.,0.,0.));
#9896=DIRECTION('',(0.,0.,1.));
#9897=DIRECTION('center_axis',(0.,0.,1.));
#9898=DIRECTION('ref_axis',(1.,0.,0.));
#9899=DIRECTION('',(1.,0.,0.));
#9900=DIRECTION('center_axis',(0.,0.,1.));
#9901=DIRECTION('ref_axis',(1.,0.,0.));
#9902=DIRECTION('center_axis',(0.,0.,1.));
#9903=DIRECTION('ref_axis',(1.,0.,0.));
#9904=DIRECTION('',(0.,0.,-1.));
#9905=DIRECTION('center_axis',(0.,0.,1.));
#9906=DIRECTION('ref_axis',(1.,0.,0.));
#9907=DIRECTION('',(0.,0.,1.));
#9908=DIRECTION('center_axis',(0.,0.,-1.));
#9909=DIRECTION('ref_axis',(1.,0.,0.));
#9910=DIRECTION('center_axis',(0.,0.,1.));
#9911=DIRECTION('ref_axis',(1.,0.,0.));
#9912=DIRECTION('',(0.,0.,1.));
#9913=DIRECTION('center_axis',(0.,-1.,0.));
#9914=DIRECTION('ref_axis',(0.,0.,-1.));
#9915=DIRECTION('',(-1.,0.,0.));
#9916=DIRECTION('',(-1.,0.,0.));
#9917=DIRECTION('',(0.,0.,1.));
#9918=DIRECTION('',(1.,0.,0.));
#9919=DIRECTION('',(0.,0.,-1.));
#9920=DIRECTION('',(-1.,0.,0.));
#9921=DIRECTION('center_axis',(0.,1.,0.));
#9922=DIRECTION('ref_axis',(0.,0.,1.));
#9923=DIRECTION('',(1.,0.,0.));
#9924=DIRECTION('',(1.,0.,0.));
#9925=DIRECTION('',(0.,0.,1.));
#9926=DIRECTION('',(1.,0.,0.));
#9927=DIRECTION('',(0.,0.,-1.));
#9928=DIRECTION('',(1.,0.,0.));
#9929=DIRECTION('center_axis',(-1.,0.,0.));
#9930=DIRECTION('ref_axis',(0.,0.,1.));
#9931=DIRECTION('',(0.,-1.,0.));
#9932=DIRECTION('',(0.,0.,1.));
#9933=DIRECTION('',(0.,1.,0.));
#9934=DIRECTION('',(0.,0.,-1.));
#9935=DIRECTION('',(0.,-1.,0.));
#9936=DIRECTION('',(0.,-1.,0.));
#9937=DIRECTION('',(0.,0.,1.));
#9938=DIRECTION('',(0.,-1.,0.));
#9939=DIRECTION('',(0.,0.,-1.));
#9940=DIRECTION('',(0.,-1.,0.));
#9941=DIRECTION('center_axis',(0.,0.,-1.));
#9942=DIRECTION('ref_axis',(0.,1.,0.));
#9943=DIRECTION('',(0.,1.,0.));
#9944=DIRECTION('',(1.,0.,0.));
#9945=DIRECTION('center_axis',(0.,-1.,0.));
#9946=DIRECTION('ref_axis',(0.,0.,-1.));
#9947=DIRECTION('',(0.,0.,-1.));
#9948=DIRECTION('',(1.,0.,0.));
#9949=DIRECTION('center_axis',(0.,0.,1.));
#9950=DIRECTION('ref_axis',(0.,-1.,0.));
#9951=DIRECTION('',(0.,-1.,0.));
#9952=DIRECTION('',(1.,0.,0.));
#9953=DIRECTION('center_axis',(0.,1.,0.));
#9954=DIRECTION('ref_axis',(0.,0.,1.));
#9955=DIRECTION('',(0.,0.,1.));
#9956=DIRECTION('',(1.,0.,0.));
#9957=DIRECTION('center_axis',(0.,0.,-1.));
#9958=DIRECTION('ref_axis',(0.,1.,0.));
#9959=DIRECTION('',(0.,1.,0.));
#9960=DIRECTION('center_axis',(0.,0.,-1.));
#9961=DIRECTION('ref_axis',(0.,1.,0.));
#9962=DIRECTION('',(0.,1.,0.));
#9963=DIRECTION('',(1.,0.,0.));
#9964=DIRECTION('center_axis',(0.,-1.,0.));
#9965=DIRECTION('ref_axis',(0.,0.,-1.));
#9966=DIRECTION('',(0.,0.,-1.));
#9967=DIRECTION('',(1.,0.,0.));
#9968=DIRECTION('center_axis',(0.,0.,-1.));
#9969=DIRECTION('ref_axis',(0.,1.,0.));
#9970=DIRECTION('',(0.,1.,0.));
#9971=DIRECTION('',(1.,0.,0.));
#9972=DIRECTION('center_axis',(0.,1.,0.));
#9973=DIRECTION('ref_axis',(0.,0.,1.));
#9974=DIRECTION('',(0.,0.,1.));
#9975=DIRECTION('',(1.,0.,0.));
#9976=DIRECTION('center_axis',(0.,0.,-1.));
#9977=DIRECTION('ref_axis',(0.,1.,0.));
#9978=DIRECTION('',(0.,1.,0.));
#9979=DIRECTION('center_axis',(1.,0.,0.));
#9980=DIRECTION('ref_axis',(0.,0.,-1.));
#9981=DIRECTION('axis',(0.,0.,1.));
#9982=DIRECTION('refdir',(1.,0.,0.));
#9983=DIRECTION('center_axis',(0.,0.,1.));
#9984=DIRECTION('ref_axis',(0.,-1.,0.));
#9985=DIRECTION('',(0.,-1.,0.));
#9986=DIRECTION('',(1.,0.,0.));
#9987=DIRECTION('',(0.,-1.,0.));
#9988=DIRECTION('',(1.,0.,0.));
#9989=DIRECTION('center_axis',(0.,1.,0.));
#9990=DIRECTION('ref_axis',(0.,0.,1.));
#9991=DIRECTION('',(0.,0.,1.));
#9992=DIRECTION('',(0.,0.,1.));
#9993=DIRECTION('',(1.,0.,0.));
#9994=DIRECTION('center_axis',(0.,0.,-1.));
#9995=DIRECTION('ref_axis',(0.,1.,0.));
#9996=DIRECTION('',(0.,1.,0.));
#9997=DIRECTION('',(0.,1.,0.));
#9998=DIRECTION('',(1.,0.,0.));
#9999=DIRECTION('center_axis',(0.,-1.,0.));
#10000=DIRECTION('ref_axis',(0.,0.,-1.));
#10001=DIRECTION('',(0.,0.,-1.));
#10002=DIRECTION('',(0.,0.,-1.));
#10003=DIRECTION('',(1.,0.,0.));
#10004=DIRECTION('center_axis',(0.,0.,-1.));
#10005=DIRECTION('ref_axis',(0.,1.,0.));
#10006=DIRECTION('',(0.,1.,0.));
#10007=DIRECTION('',(0.,1.,0.));
#10008=DIRECTION('',(1.,0.,0.));
#10009=DIRECTION('center_axis',(0.,1.,0.));
#10010=DIRECTION('ref_axis',(0.,0.,1.));
#10011=DIRECTION('',(0.,0.,1.));
#10012=DIRECTION('',(0.,0.,1.));
#10013=DIRECTION('',(1.,0.,0.));
#10014=DIRECTION('center_axis',(0.,0.,-1.));
#10015=DIRECTION('ref_axis',(0.,1.,0.));
#10016=DIRECTION('',(0.,1.,0.));
#10017=DIRECTION('',(0.,1.,0.));
#10018=DIRECTION('',(1.,0.,0.));
#10019=DIRECTION('center_axis',(0.,-1.,0.));
#10020=DIRECTION('ref_axis',(0.,0.,-1.));
#10021=DIRECTION('',(0.,0.,-1.));
#10022=DIRECTION('',(0.,0.,-1.));
#10023=DIRECTION('center_axis',(1.,0.,0.));
#10024=DIRECTION('ref_axis',(0.,0.,-1.));
#10025=DIRECTION('center_axis',(1.,0.,0.));
#10026=DIRECTION('ref_axis',(0.,0.,-1.));
#10027=DIRECTION('axis',(0.,0.,1.));
#10028=DIRECTION('refdir',(1.,0.,0.));
#10029=DIRECTION('center_axis',(0.,0.,-1.));
#10030=DIRECTION('ref_axis',(0.,-1.,0.));
#10031=DIRECTION('',(0.,1.,0.));
#10032=DIRECTION('',(-1.,0.,0.));
#10033=DIRECTION('',(0.,-1.,0.));
#10034=DIRECTION('',(-1.,0.,0.));
#10035=DIRECTION('center_axis',(0.,1.,0.));
#10036=DIRECTION('ref_axis',(0.,0.,-1.));
#10037=DIRECTION('',(0.,0.,1.));
#10038=DIRECTION('',(0.,0.,-1.));
#10039=DIRECTION('',(-1.,0.,0.));
#10040=DIRECTION('center_axis',(0.,0.,-1.));
#10041=DIRECTION('ref_axis',(0.,-1.,0.));
#10042=DIRECTION('',(0.,1.,0.));
#10043=DIRECTION('',(0.,-1.,0.));
#10044=DIRECTION('',(-1.,0.,0.));
#10045=DIRECTION('center_axis',(0.,-1.,0.));
#10046=DIRECTION('ref_axis',(0.,0.,1.));
#10047=DIRECTION('',(0.,0.,-1.));
#10048=DIRECTION('',(0.,0.,1.));
#10049=DIRECTION('',(-1.,0.,0.));
#10050=DIRECTION('center_axis',(0.,0.,-1.));
#10051=DIRECTION('ref_axis',(0.,-1.,0.));
#10052=DIRECTION('',(0.,1.,0.));
#10053=DIRECTION('',(0.,-1.,0.));
#10054=DIRECTION('',(-1.,0.,0.));
#10055=DIRECTION('center_axis',(0.,1.,0.));
#10056=DIRECTION('ref_axis',(0.,0.,-1.));
#10057=DIRECTION('',(0.,0.,1.));
#10058=DIRECTION('',(0.,0.,-1.));
#10059=DIRECTION('',(-1.,0.,0.));
#10060=DIRECTION('center_axis',(0.,0.,1.));
#10061=DIRECTION('ref_axis',(0.,1.,0.));
#10062=DIRECTION('',(0.,-1.,0.));
#10063=DIRECTION('',(0.,1.,0.));
#10064=DIRECTION('',(-1.,0.,0.));
#10065=DIRECTION('center_axis',(0.,-1.,0.));
#10066=DIRECTION('ref_axis',(0.,0.,1.));
#10067=DIRECTION('',(0.,0.,-1.));
#10068=DIRECTION('',(0.,0.,1.));
#10069=DIRECTION('center_axis',(1.,0.,0.));
#10070=DIRECTION('ref_axis',(0.,0.,-1.));
#10071=DIRECTION('center_axis',(-1.,0.,0.));
#10072=DIRECTION('ref_axis',(0.,0.,1.));
#10073=DIRECTION('',(0.,0.,1.));
#10074=DIRECTION('',(1.,0.,0.));
#10075=DIRECTION('',(0.,0.,1.));
#10076=DIRECTION('',(1.,0.,0.));
#10077=DIRECTION('',(0.,0.,1.));
#10078=DIRECTION('',(1.,0.,0.));
#10079=DIRECTION('axis',(0.,0.,1.));
#10080=DIRECTION('refdir',(1.,0.,0.));
#10081=DIRECTION('center_axis',(0.866025403784439,0.,-0.5));
#10082=DIRECTION('ref_axis',(0.5,0.,0.866025403784439));
#10083=DIRECTION('',(-0.5,0.,-0.866025403784439));
#10084=DIRECTION('',(0.,-1.,0.));
#10085=DIRECTION('',(0.5,0.,0.866025403784439));
#10086=DIRECTION('',(0.,-1.,0.));
#10087=DIRECTION('center_axis',(1.20185167898973E-16,0.,-1.));
#10088=DIRECTION('ref_axis',(1.,0.,1.20185167898973E-16));
#10089=DIRECTION('',(-1.,0.,-1.20185167898973E-16));
#10090=DIRECTION('',(0.,-1.,0.));
#10091=DIRECTION('',(1.,0.,1.20185167898973E-16));
#10092=DIRECTION('center_axis',(-0.866025403784439,0.,-0.5));
#10093=DIRECTION('ref_axis',(0.5,0.,-0.866025403784439));
#10094=DIRECTION('',(-0.5,0.,0.866025403784439));
#10095=DIRECTION('',(0.,-1.,0.));
#10096=DIRECTION('',(0.5,0.,-0.866025403784439));
#10097=DIRECTION('center_axis',(-0.866025403784439,0.,0.5));
#10098=DIRECTION('ref_axis',(-0.5,0.,-0.866025403784439));
#10099=DIRECTION('',(0.5,0.,0.866025403784439));
#10100=DIRECTION('',(0.,-1.,0.));
#10101=DIRECTION('',(-0.5,0.,-0.866025403784439));
#10102=DIRECTION('center_axis',(-2.40370335797945E-16,0.,1.));
#10103=DIRECTION('ref_axis',(-1.,0.,-2.40370335797945E-16));
#10104=DIRECTION('',(1.,0.,2.40370335797945E-16));
#10105=DIRECTION('',(0.,-1.,0.));
#10106=DIRECTION('',(-1.,0.,-2.40370335797945E-16));
#10107=DIRECTION('center_axis',(0.866025403784439,0.,0.5));
#10108=DIRECTION('ref_axis',(-0.5,0.,0.866025403784439));
#10109=DIRECTION('',(0.5,0.,-0.866025403784439));
#10110=DIRECTION('',(-0.5,0.,0.866025403784439));
#10111=DIRECTION('center_axis',(0.,1.,0.));
#10112=DIRECTION('ref_axis',(1.,0.,0.));
#10113=DIRECTION('center_axis',(0.,-1.,0.));
#10114=DIRECTION('ref_axis',(0.,0.,-1.));
#10115=DIRECTION('center_axis',(0.,1.,0.));
#10116=DIRECTION('ref_axis',(1.,0.,0.));
#10117=DIRECTION('center_axis',(0.,1.,0.));
#10118=DIRECTION('ref_axis',(1.,0.,0.));
#10119=DIRECTION('center_axis',(0.,1.,0.));
#10120=DIRECTION('ref_axis',(0.,0.,1.));
#10121=DIRECTION('center_axis',(0.,-1.,0.));
#10122=DIRECTION('ref_axis',(1.,0.,0.));
#10123=DIRECTION('center_axis',(0.,-1.,0.));
#10124=DIRECTION('ref_axis',(1.,0.,0.));
#10125=DIRECTION('center_axis',(0.,-1.,0.));
#10126=DIRECTION('ref_axis',(1.,0.,0.));
#10127=DIRECTION('',(0.707106781186548,0.707106781186547,8.65956056235493E-17));
#10128=DIRECTION('center_axis',(0.,-1.,0.));
#10129=DIRECTION('ref_axis',(1.,0.,0.));
#10130=DIRECTION('center_axis',(0.,-1.,0.));
#10131=DIRECTION('ref_axis',(1.,0.,0.));
#10132=DIRECTION('',(0.,1.,0.));
#10133=DIRECTION('center_axis',(0.,1.,0.));
#10134=DIRECTION('ref_axis',(1.,0.,0.));
#10135=DIRECTION('center_axis',(0.,-1.,0.));
#10136=DIRECTION('ref_axis',(1.,0.,0.));
#10137=DIRECTION('',(-0.707106781186547,0.707106781186548,-8.65956056235493E-17));
#10138=DIRECTION('center_axis',(0.,-1.,0.));
#10139=DIRECTION('ref_axis',(0.,0.,-1.));
#10140=DIRECTION('center_axis',(0.,-1.,0.));
#10141=DIRECTION('ref_axis',(1.,0.,0.));
#10142=DIRECTION('center_axis',(0.,1.,0.));
#10143=DIRECTION('ref_axis',(1.,0.,0.));
#10144=DIRECTION('center_axis',(0.,1.,0.));
#10145=DIRECTION('ref_axis',(1.,0.,0.));
#10146=DIRECTION('',(-0.447213595499958,0.894427190999916,-5.47678698264203E-17));
#10147=DIRECTION('center_axis',(0.,-1.,0.));
#10148=DIRECTION('ref_axis',(1.,0.,0.));
#10149=DIRECTION('',(0.,1.,0.));
#10150=DIRECTION('axis',(0.,0.,1.));
#10151=DIRECTION('refdir',(1.,0.,0.));
#10152=DIRECTION('center_axis',(0.,1.,0.));
#10153=DIRECTION('ref_axis',(0.,0.,1.));
#10154=DIRECTION('center_axis',(0.,-1.,0.));
#10155=DIRECTION('ref_axis',(1.,0.,0.));
#10156=DIRECTION('center_axis',(0.,-1.,0.));
#10157=DIRECTION('ref_axis',(1.,0.,0.));
#10158=DIRECTION('center_axis',(0.,-1.,0.));
#10159=DIRECTION('ref_axis',(1.,0.,0.));
#10160=DIRECTION('',(0.707106781186547,0.707106781186548,8.65956056235493E-17));
#10161=DIRECTION('center_axis',(0.,-1.,0.));
#10162=DIRECTION('ref_axis',(1.,0.,0.));
#10163=DIRECTION('center_axis',(0.,-1.,0.));
#10164=DIRECTION('ref_axis',(1.,0.,0.));
#10165=DIRECTION('',(0.,1.,0.));
#10166=DIRECTION('center_axis',(0.,1.,0.));
#10167=DIRECTION('ref_axis',(1.,0.,0.));
#10168=DIRECTION('center_axis',(0.,-1.,0.));
#10169=DIRECTION('ref_axis',(1.,0.,0.));
#10170=DIRECTION('',(-0.707106781186547,0.707106781186548,-8.65956056235493E-17));
#10171=DIRECTION('center_axis',(0.,-1.,0.));
#10172=DIRECTION('ref_axis',(0.,0.,-1.));
#10173=DIRECTION('center_axis',(0.,-1.,0.));
#10174=DIRECTION('ref_axis',(1.,0.,0.));
#10175=DIRECTION('center_axis',(0.,1.,0.));
#10176=DIRECTION('ref_axis',(1.,0.,0.));
#10177=DIRECTION('center_axis',(0.,1.,0.));
#10178=DIRECTION('ref_axis',(1.,0.,0.));
#10179=DIRECTION('',(-0.447213595499958,0.894427190999916,-5.47678698264203E-17));
#10180=DIRECTION('center_axis',(0.,-1.,0.));
#10181=DIRECTION('ref_axis',(1.,0.,0.));
#10182=DIRECTION('center_axis',(0.,1.,0.));
#10183=DIRECTION('ref_axis',(1.,0.,0.));
#10184=DIRECTION('',(0.,1.,0.));
#10185=DIRECTION('center_axis',(0.,1.,0.));
#10186=DIRECTION('ref_axis',(1.,0.,0.));
#10187=DIRECTION('center_axis',(0.,-1.,0.));
#10188=DIRECTION('ref_axis',(1.,0.,0.));
#10189=DIRECTION('',(-0.707106781186547,0.707106781186548,-8.65956056235493E-17));
#10190=DIRECTION('center_axis',(0.,-1.,0.));
#10191=DIRECTION('ref_axis',(0.,0.,-1.));
#10192=DIRECTION('center_axis',(0.866025403784439,0.,-0.5));
#10193=DIRECTION('ref_axis',(0.5,0.,0.866025403784439));
#10194=DIRECTION('',(-0.5,0.,-0.866025403784439));
#10195=DIRECTION('',(0.,-1.,0.));
#10196=DIRECTION('',(0.5,0.,0.866025403784439));
#10197=DIRECTION('',(0.,-1.,0.));
#10198=DIRECTION('center_axis',(1.60246890531964E-16,0.,-1.));
#10199=DIRECTION('ref_axis',(1.,0.,1.60246890531964E-16));
#10200=DIRECTION('',(-1.,0.,-1.60246890531964E-16));
#10201=DIRECTION('',(0.,-1.,0.));
#10202=DIRECTION('',(1.,0.,1.60246890531964E-16));
#10203=DIRECTION('center_axis',(-0.866025403784439,0.,-0.5));
#10204=DIRECTION('ref_axis',(0.5,0.,-0.866025403784439));
#10205=DIRECTION('',(-0.5,0.,0.866025403784439));
#10206=DIRECTION('',(0.,-1.,0.));
#10207=DIRECTION('',(0.5,0.,-0.866025403784439));
#10208=DIRECTION('center_axis',(-0.866025403784439,0.,0.5));
#10209=DIRECTION('ref_axis',(-0.5,0.,-0.866025403784439));
#10210=DIRECTION('',(0.5,0.,0.866025403784439));
#10211=DIRECTION('',(0.,-1.,0.));
#10212=DIRECTION('',(-0.5,0.,-0.866025403784439));
#10213=DIRECTION('center_axis',(-1.60246890531964E-16,0.,1.));
#10214=DIRECTION('ref_axis',(-1.,0.,-1.60246890531964E-16));
#10215=DIRECTION('',(1.,0.,1.60246890531964E-16));
#10216=DIRECTION('',(0.,-1.,0.));
#10217=DIRECTION('',(-1.,0.,-1.60246890531964E-16));
#10218=DIRECTION('center_axis',(0.866025403784439,0.,0.5));
#10219=DIRECTION('ref_axis',(-0.5,0.,0.866025403784439));
#10220=DIRECTION('',(0.5,0.,-0.866025403784439));
#10221=DIRECTION('',(-0.5,0.,0.866025403784439));
#10222=DIRECTION('center_axis',(0.,1.,0.));
#10223=DIRECTION('ref_axis',(1.,0.,0.));
#10224=DIRECTION('center_axis',(0.,-1.,0.));
#10225=DIRECTION('ref_axis',(0.,0.,-1.));
#10226=DIRECTION('',(0.,0.,1.));
#10227=DIRECTION('',(1.,0.,0.));
#10228=DIRECTION('',(0.,0.,1.));
#10229=DIRECTION('',(1.,0.,0.));
#10230=DIRECTION('',(0.,0.,1.));
#10231=DIRECTION('',(1.,0.,0.));
#10232=DIRECTION('',(0.,0.,1.));
#10233=DIRECTION('',(1.,0.,0.));
#10234=DIRECTION('',(0.,0.,1.));
#10235=DIRECTION('',(1.,0.,0.));
#10236=DIRECTION('',(0.,0.,1.));
#10237=DIRECTION('',(1.,0.,0.));
#10238=DIRECTION('',(0.,0.,1.));
#10239=DIRECTION('',(1.,0.,0.));
#10240=DIRECTION('',(0.,0.,1.));
#10241=DIRECTION('',(1.,0.,0.));
#10242=DIRECTION('',(0.,0.,1.));
#10243=DIRECTION('',(1.,0.,0.));
#10244=DIRECTION('',(0.,0.,1.));
#10245=DIRECTION('',(1.,0.,0.));
#10246=DIRECTION('',(0.,0.,1.));
#10247=DIRECTION('',(1.,0.,0.));
#10248=DIRECTION('',(0.,0.,1.));
#10249=DIRECTION('',(1.,0.,0.));
#10250=DIRECTION('',(0.,0.,1.));
#10251=DIRECTION('',(1.,0.,0.));
#10252=DIRECTION('',(0.,0.,1.));
#10253=DIRECTION('',(1.,0.,0.));
#10254=DIRECTION('',(0.,0.,1.));
#10255=DIRECTION('',(1.,0.,0.));
#10256=DIRECTION('',(0.,0.,1.));
#10257=DIRECTION('',(1.,0.,0.));
#10258=DIRECTION('',(0.,0.,1.));
#10259=DIRECTION('',(1.,0.,0.));
#10260=DIRECTION('',(-1.,0.,2.22044604925031E-16));
#10261=DIRECTION('',(2.22044604925031E-16,0.,1.));
#10262=DIRECTION('',(0.,1.,2.22044604925031E-16));
#10263=DIRECTION('',(1.,0.,0.));
#10264=DIRECTION('',(0.,-1.,2.22044604925031E-16));
#10265=DIRECTION('',(1.,0.,0.));
#10266=DIRECTION('',(-1.,0.,2.22044604925031E-16));
#10267=DIRECTION('',(2.22044604925031E-16,0.,1.));
#10268=DIRECTION('',(0.,0.,1.));
#10269=DIRECTION('',(2.22044604925031E-16,1.,0.));
#10270=DIRECTION('',(0.,0.,1.));
#10271=DIRECTION('',(2.22044604925031E-16,1.,0.));
#10272=DIRECTION('',(-1.,0.,2.22044604925031E-16));
#10273=DIRECTION('',(2.22044604925031E-16,0.,1.));
#10274=DIRECTION('',(0.,0.,1.));
#10275=DIRECTION('',(2.22044604925031E-16,1.,0.));
#10276=DIRECTION('',(0.,0.,1.));
#10277=DIRECTION('',(2.22044604925031E-16,1.,0.));
#10278=DIRECTION('',(-1.,0.,2.22044604925031E-16));
#10279=DIRECTION('',(2.22044604925031E-16,0.,1.));
#10280=DIRECTION('',(0.,0.,1.));
#10281=DIRECTION('',(2.22044604925031E-16,1.,0.));
#10282=DIRECTION('',(0.,0.,1.));
#10283=DIRECTION('',(2.22044604925031E-16,1.,0.));
#10284=DIRECTION('',(0.,0.,1.));
#10285=DIRECTION('',(2.22044604925031E-16,1.,0.));
#10286=DIRECTION('',(0.,0.,1.));
#10287=DIRECTION('',(2.22044604925031E-16,1.,0.));
#10288=DIRECTION('',(0.,0.,1.));
#10289=DIRECTION('',(2.22044604925031E-16,1.,0.));
#10290=DIRECTION('',(0.,0.,1.));
#10291=DIRECTION('',(2.22044604925031E-16,1.,0.));
#10292=DIRECTION('',(0.,-1.,2.22044604925031E-16));
#10293=DIRECTION('',(1.,0.,0.));
#10294=DIRECTION('',(0.,-1.,0.));
#10295=DIRECTION('',(0.,0.,-1.));
#10296=DIRECTION('',(0.,0.,1.));
#10297=DIRECTION('',(-1.,1.22464679914735E-16,0.));
#10298=DIRECTION('',(0.,0.,1.));
#10299=DIRECTION('',(-1.,1.22464679914735E-16,0.));
#10300=DIRECTION('',(0.,-1.,2.22044604925031E-16));
#10301=DIRECTION('',(1.,0.,0.));
#10302=DIRECTION('',(0.,1.,0.));
#10303=DIRECTION('',(0.,0.,1.));
#10304=DIRECTION('',(0.,0.,1.));
#10305=DIRECTION('',(1.,0.,0.));
#10306=DIRECTION('',(0.,0.,1.));
#10307=DIRECTION('',(1.,0.,0.));
#10308=DIRECTION('',(0.,0.,1.));
#10309=DIRECTION('',(1.,0.,0.));
#10310=DIRECTION('',(0.,0.,1.));
#10311=DIRECTION('',(1.,0.,0.));
#10312=DIRECTION('',(0.,0.,1.));
#10313=DIRECTION('',(1.,0.,0.));
#10314=DIRECTION('',(0.,0.,1.));
#10315=DIRECTION('',(1.,0.,0.));
#10316=DIRECTION('',(0.,0.,1.));
#10317=DIRECTION('',(1.,0.,0.));
#10318=DIRECTION('',(0.,0.,1.));
#10319=DIRECTION('',(1.,0.,0.));
#10320=DIRECTION('',(0.,0.,1.));
#10321=DIRECTION('',(1.,0.,0.));
#10322=DIRECTION('',(-1.,0.,2.22044604925031E-16));
#10323=DIRECTION('',(2.22044604925031E-16,0.,1.));
#10324=DIRECTION('',(0.,0.,1.));
#10325=DIRECTION('',(2.22044604925031E-16,1.,0.));
#10326=DIRECTION('',(0.,0.,1.));
#10327=DIRECTION('',(2.22044604925031E-16,1.,0.));
#10328=DIRECTION('',(0.,0.,1.));
#10329=DIRECTION('',(2.22044604925031E-16,1.,0.));
#10330=DIRECTION('',(0.,0.,1.));
#10331=DIRECTION('',(2.22044604925031E-16,1.,0.));
#10332=DIRECTION('',(0.,0.,1.));
#10333=DIRECTION('',(2.22044604925031E-16,1.,0.));
#10334=DIRECTION('',(0.,0.,1.));
#10335=DIRECTION('',(1.,0.,0.));
#10336=DIRECTION('',(6.12323399573673E-17,4.3815077841081E-81,1.));
#10337=DIRECTION('',(1.,2.8115992571124E-65,-6.12323399573677E-17));
#10338=CARTESIAN_POINT('',(0.,0.,0.));
#10339=CARTESIAN_POINT('',(0.,0.,0.));
#10340=CARTESIAN_POINT('',(0.,0.,0.));
#10341=CARTESIAN_POINT('Origin',(3.,3.5,-0.9));
#10342=CARTESIAN_POINT('',(2.79,3.5,-0.9));
#10343=CARTESIAN_POINT('Origin',(3.,3.5,-0.9));
#10344=CARTESIAN_POINT('',(2.79,3.5,0.));
#10345=CARTESIAN_POINT('',(2.79,3.5,-0.9));
#10346=CARTESIAN_POINT('Origin',(3.,3.5,0.));
#10347=CARTESIAN_POINT('Origin',(3.,3.5,-0.9));
#10348=CARTESIAN_POINT('Origin',(3.,-3.5,-0.9));
#10349=CARTESIAN_POINT('',(2.79,-3.5,-0.9));
#10350=CARTESIAN_POINT('Origin',(3.,-3.5,-0.9));
#10351=CARTESIAN_POINT('',(2.79,-3.5,0.));
#10352=CARTESIAN_POINT('',(2.79,-3.5,-0.9));
#10353=CARTESIAN_POINT('Origin',(3.,-3.5,0.));
#10354=CARTESIAN_POINT('Origin',(3.,-3.5,-0.9));
#10355=CARTESIAN_POINT('Origin',(-5.2,0.,-0.9));
#10356=CARTESIAN_POINT('',(-5.365,-2.02066721859313E-17,-0.9));
#10357=CARTESIAN_POINT('Origin',(-5.2,0.,-0.9));
#10358=CARTESIAN_POINT('',(-5.365,2.02066721859313E-17,0.));
#10359=CARTESIAN_POINT('',(-5.365,-2.02066721859313E-17,-0.9));
#10360=CARTESIAN_POINT('Origin',(-5.2,0.,0.));
#10361=CARTESIAN_POINT('Origin',(-5.2,0.,-0.9));
#10362=CARTESIAN_POINT('Origin',(-8.8,0.,-0.9));
#10363=CARTESIAN_POINT('',(-8.965,-2.02066721859312E-17,-0.9));
#10364=CARTESIAN_POINT('Origin',(-8.8,0.,-0.9));
#10365=CARTESIAN_POINT('',(-8.965,2.02066721859312E-17,0.));
#10366=CARTESIAN_POINT('',(-8.965,-2.02066721859312E-17,-0.9));
#10367=CARTESIAN_POINT('Origin',(-8.8,0.,0.));
#10368=CARTESIAN_POINT('Origin',(-8.8,0.,-0.9));
#10369=CARTESIAN_POINT('Origin',(3.,0.,-1.1));
#10370=CARTESIAN_POINT('',(2.725,-3.36777869765522E-17,-1.));
#10371=CARTESIAN_POINT('Origin',(3.,0.,-1.));
#10372=CARTESIAN_POINT('',(2.725,3.36777869765522E-17,0.));
#10373=CARTESIAN_POINT('',(2.725,-3.36777869765522E-17,-1.1));
#10374=CARTESIAN_POINT('Origin',(3.,0.,0.));
#10375=CARTESIAN_POINT('Origin',(6.,6.,-1.));
#10376=CARTESIAN_POINT('',(6.,6.,-1.));
#10377=CARTESIAN_POINT('',(-12.,6.,-1.));
#10378=CARTESIAN_POINT('',(6.,6.,-1.));
#10379=CARTESIAN_POINT('',(-12.,6.,0.));
#10380=CARTESIAN_POINT('',(-12.,6.,-1.));
#10381=CARTESIAN_POINT('',(6.,6.,0.));
#10382=CARTESIAN_POINT('',(6.,6.,0.));
#10383=CARTESIAN_POINT('',(6.,6.,-1.));
#10384=CARTESIAN_POINT('Origin',(6.,-6.,-1.));
#10385=CARTESIAN_POINT('',(6.,-6.,-1.));
#10386=CARTESIAN_POINT('',(6.,-6.,-1.));
#10387=CARTESIAN_POINT('',(6.,-6.,0.));
#10388=CARTESIAN_POINT('',(6.,-6.,0.));
#10389=CARTESIAN_POINT('',(6.,-6.,-1.));
#10390=CARTESIAN_POINT('Origin',(-12.,-6.,-1.));
#10391=CARTESIAN_POINT('',(-12.,-6.,-1.));
#10392=CARTESIAN_POINT('',(-12.,-6.,-1.));
#10393=CARTESIAN_POINT('',(-12.,-6.,0.));
#10394=CARTESIAN_POINT('',(-12.,-6.,0.));
#10395=CARTESIAN_POINT('',(-12.,-6.,-1.));
#10396=CARTESIAN_POINT('Origin',(-12.,6.,-1.));
#10397=CARTESIAN_POINT('',(-12.,6.,-1.));
#10398=CARTESIAN_POINT('',(-12.,6.,0.));
#10399=CARTESIAN_POINT('Origin',(-3.,0.,0.));
#10400=CARTESIAN_POINT('Origin',(-3.,0.,-1.));
#10401=CARTESIAN_POINT('',(0.,0.,0.));
#10402=CARTESIAN_POINT('Origin',(6.,-5.,-1.8));
#10403=CARTESIAN_POINT('',(6.,-5.,-1.8));
#10404=CARTESIAN_POINT('',(-12.,-5.,-1.8));
#10405=CARTESIAN_POINT('',(6.,-5.,-1.8));
#10406=CARTESIAN_POINT('',(-12.,-5.,-1.));
#10407=CARTESIAN_POINT('',(-12.,-5.,-1.8));
#10408=CARTESIAN_POINT('',(6.,-5.,-1.));
#10409=CARTESIAN_POINT('',(6.,-5.,-1.));
#10410=CARTESIAN_POINT('',(6.,-5.,-1.8));
#10411=CARTESIAN_POINT('Origin',(6.,-6.,-1.8));
#10412=CARTESIAN_POINT('',(6.,-6.,-1.8));
#10413=CARTESIAN_POINT('',(6.,-6.,-1.8));
#10414=CARTESIAN_POINT('',(6.,-6.,-1.));
#10415=CARTESIAN_POINT('',(6.,-6.,-1.));
#10416=CARTESIAN_POINT('',(6.,-6.,-1.8));
#10417=CARTESIAN_POINT('Origin',(-12.,-6.,-1.8));
#10418=CARTESIAN_POINT('',(-12.,-6.,-1.8));
#10419=CARTESIAN_POINT('',(-12.,-6.,-1.8));
#10420=CARTESIAN_POINT('',(-12.,-6.,-1.));
#10421=CARTESIAN_POINT('',(-12.,-6.,-1.));
#10422=CARTESIAN_POINT('',(-12.,-6.,-1.8));
#10423=CARTESIAN_POINT('Origin',(-12.,-5.,-1.8));
#10424=CARTESIAN_POINT('',(-12.,-5.,-1.8));
#10425=CARTESIAN_POINT('',(-12.,-5.,-1.));
#10426=CARTESIAN_POINT('Origin',(-3.,-5.5,-1.));
#10427=CARTESIAN_POINT('Origin',(-3.,-5.5,-1.8));
#10428=CARTESIAN_POINT('',(0.,0.,0.));
#10429=CARTESIAN_POINT('Origin',(6.,6.,-1.8));
#10430=CARTESIAN_POINT('',(6.,6.,-1.8));
#10431=CARTESIAN_POINT('',(-12.,6.,-1.8));
#10432=CARTESIAN_POINT('',(6.,6.,-1.8));
#10433=CARTESIAN_POINT('',(-12.,6.,-1.));
#10434=CARTESIAN_POINT('',(-12.,6.,-1.8));
#10435=CARTESIAN_POINT('',(6.,6.,-1.));
#10436=CARTESIAN_POINT('',(6.,6.,-1.));
#10437=CARTESIAN_POINT('',(6.,6.,-1.8));
#10438=CARTESIAN_POINT('Origin',(6.,5.,-1.8));
#10439=CARTESIAN_POINT('',(6.,5.,-1.8));
#10440=CARTESIAN_POINT('',(6.,5.,-1.8));
#10441=CARTESIAN_POINT('',(6.,5.,-1.));
#10442=CARTESIAN_POINT('',(6.,5.,-1.));
#10443=CARTESIAN_POINT('',(6.,5.,-1.8));
#10444=CARTESIAN_POINT('Origin',(-12.,5.,-1.8));
#10445=CARTESIAN_POINT('',(-12.,5.,-1.8));
#10446=CARTESIAN_POINT('',(-12.,5.,-1.8));
#10447=CARTESIAN_POINT('',(-12.,5.,-1.));
#10448=CARTESIAN_POINT('',(-12.,5.,-1.));
#10449=CARTESIAN_POINT('',(-12.,5.,-1.8));
#10450=CARTESIAN_POINT('Origin',(-12.,6.,-1.8));
#10451=CARTESIAN_POINT('',(-12.,6.,-1.8));
#10452=CARTESIAN_POINT('',(-12.,6.,-1.));
#10453=CARTESIAN_POINT('Origin',(-3.,5.5,-1.));
#10454=CARTESIAN_POINT('Origin',(-3.,5.5,-1.8));
#10455=CARTESIAN_POINT('',(0.,0.,0.));
#10456=CARTESIAN_POINT('Origin',(3.,0.,39.9));
#10457=CARTESIAN_POINT('',(2.725,-3.36777869765522E-17,40.));
#10458=CARTESIAN_POINT('Origin',(3.,0.,40.));
#10459=CARTESIAN_POINT('',(2.725,3.36777869765522E-17,40.8));
#10460=CARTESIAN_POINT('',(2.725,-3.36777869765522E-17,39.9));
#10461=CARTESIAN_POINT('Origin',(3.,0.,40.8));
#10462=CARTESIAN_POINT('Origin',(4.,1.,40.));
#10463=CARTESIAN_POINT('',(4.,1.,40.));
#10464=CARTESIAN_POINT('',(2.,1.,40.));
#10465=CARTESIAN_POINT('',(4.,1.,40.));
#10466=CARTESIAN_POINT('',(2.,1.,40.8));
#10467=CARTESIAN_POINT('',(2.,1.,40.));
#10468=CARTESIAN_POINT('',(4.,1.,40.8));
#10469=CARTESIAN_POINT('',(4.,1.,40.8));
#10470=CARTESIAN_POINT('',(4.,1.,40.));
#10471=CARTESIAN_POINT('Origin',(4.,-1.,40.));
#10472=CARTESIAN_POINT('',(4.,-1.,40.));
#10473=CARTESIAN_POINT('',(4.,-1.,40.));
#10474=CARTESIAN_POINT('',(4.,-1.,40.8));
#10475=CARTESIAN_POINT('',(4.,-1.,40.8));
#10476=CARTESIAN_POINT('',(4.,-1.,40.));
#10477=CARTESIAN_POINT('Origin',(2.,-1.,40.));
#10478=CARTESIAN_POINT('',(2.,-1.,40.));
#10479=CARTESIAN_POINT('',(2.,-1.,40.));
#10480=CARTESIAN_POINT('',(2.,-1.,40.8));
#10481=CARTESIAN_POINT('',(2.,-1.,40.8));
#10482=CARTESIAN_POINT('',(2.,-1.,40.));
#10483=CARTESIAN_POINT('Origin',(2.,1.,40.));
#10484=CARTESIAN_POINT('',(2.,1.,40.));
#10485=CARTESIAN_POINT('',(2.,1.,40.8));
#10486=CARTESIAN_POINT('Origin',(3.,0.,40.8));
#10487=CARTESIAN_POINT('Origin',(3.,0.,40.));
#10488=CARTESIAN_POINT('',(0.,0.,0.));
#10489=CARTESIAN_POINT('Origin',(1.1,2.,33.45));
#10490=CARTESIAN_POINT('',(1.2,2.,33.66));
#10491=CARTESIAN_POINT('Origin',(1.2,2.,33.45));
#10492=CARTESIAN_POINT('',(2.,2.,33.66));
#10493=CARTESIAN_POINT('',(1.1,2.,33.66));
#10494=CARTESIAN_POINT('Origin',(2.,2.,33.45));
#10495=CARTESIAN_POINT('Origin',(1.1,2.,15.55));
#10496=CARTESIAN_POINT('',(1.2,2.,15.76));
#10497=CARTESIAN_POINT('Origin',(1.2,2.,15.55));
#10498=CARTESIAN_POINT('',(2.,2.,15.76));
#10499=CARTESIAN_POINT('',(1.1,2.,15.76));
#10500=CARTESIAN_POINT('Origin',(2.,2.,15.55));
#10501=CARTESIAN_POINT('Origin',(1.1,0.,36.));
#10502=CARTESIAN_POINT('',(1.2,-2.02066721859312E-17,36.165));
#10503=CARTESIAN_POINT('Origin',(1.2,0.,36.));
#10504=CARTESIAN_POINT('',(2.,2.02066721859312E-17,36.165));
#10505=CARTESIAN_POINT('',(1.1,-2.02066721859312E-17,36.165));
#10506=CARTESIAN_POINT('Origin',(2.,0.,36.));
#10507=CARTESIAN_POINT('Origin',(1.1,0.,30.));
#10508=CARTESIAN_POINT('',(1.2,-2.02066721859312E-17,30.165));
#10509=CARTESIAN_POINT('Origin',(1.2,0.,30.));
#10510=CARTESIAN_POINT('',(2.,2.02066721859312E-17,30.165));
#10511=CARTESIAN_POINT('',(1.1,-2.02066721859312E-17,30.165));
#10512=CARTESIAN_POINT('Origin',(2.,0.,30.));
#10513=CARTESIAN_POINT('Origin',(1.1,0.,24.));
#10514=CARTESIAN_POINT('',(1.2,-2.02066721859312E-17,24.165));
#10515=CARTESIAN_POINT('Origin',(1.2,0.,24.));
#10516=CARTESIAN_POINT('',(2.,2.02066721859312E-17,24.165));
#10517=CARTESIAN_POINT('',(1.1,-2.02066721859312E-17,24.165));
#10518=CARTESIAN_POINT('Origin',(2.,0.,24.));
#10519=CARTESIAN_POINT('Origin',(1.1,0.,18.));
#10520=CARTESIAN_POINT('',(1.2,-2.02066721859312E-17,18.165));
#10521=CARTESIAN_POINT('Origin',(1.2,0.,18.));
#10522=CARTESIAN_POINT('',(2.,2.02066721859312E-17,18.165));
#10523=CARTESIAN_POINT('',(1.1,-2.02066721859312E-17,18.165));
#10524=CARTESIAN_POINT('Origin',(2.,0.,18.));
#10525=CARTESIAN_POINT('Origin',(1.1,0.,39.));
#10526=CARTESIAN_POINT('',(1.2,-3.3677786976552E-17,39.275));
#10527=CARTESIAN_POINT('Origin',(1.2,0.,39.));
#10528=CARTESIAN_POINT('',(2.,3.3677786976552E-17,39.275));
#10529=CARTESIAN_POINT('',(1.1,-3.3677786976552E-17,39.275));
#10530=CARTESIAN_POINT('Origin',(2.,0.,39.));
#10531=CARTESIAN_POINT('Origin',(1.1,0.,14.5));
#10532=CARTESIAN_POINT('',(1.2,-3.36777869765523E-17,14.775));
#10533=CARTESIAN_POINT('Origin',(1.2,0.,14.5));
#10534=CARTESIAN_POINT('',(2.,3.36777869765523E-17,14.775));
#10535=CARTESIAN_POINT('',(1.1,-3.36777869765523E-17,14.775));
#10536=CARTESIAN_POINT('Origin',(2.,0.,14.5));
#10537=CARTESIAN_POINT('Origin',(1.1,3.1,32.5));
#10538=CARTESIAN_POINT('',(2.,1.,32.5));
#10539=CARTESIAN_POINT('',(2.,3.,32.5));
#10540=CARTESIAN_POINT('',(2.,0.05,32.5));
#10541=CARTESIAN_POINT('',(1.2,1.,32.5));
#10542=CARTESIAN_POINT('',(1.1,1.,32.5));
#10543=CARTESIAN_POINT('',(1.2,3.,32.5));
#10544=CARTESIAN_POINT('',(1.2,3.05,32.5));
#10545=CARTESIAN_POINT('',(1.55,3.,32.5));
#10546=CARTESIAN_POINT('Origin',(1.1,1.,16.5));
#10547=CARTESIAN_POINT('',(2.,3.,16.5));
#10548=CARTESIAN_POINT('',(2.,1.,16.5));
#10549=CARTESIAN_POINT('',(2.,-1.,16.5));
#10550=CARTESIAN_POINT('',(1.2,3.,16.5));
#10551=CARTESIAN_POINT('',(1.55,3.,16.5));
#10552=CARTESIAN_POINT('',(1.2,1.,16.5));
#10553=CARTESIAN_POINT('',(1.2,2.,16.5));
#10554=CARTESIAN_POINT('',(1.1,1.,16.5));
#10555=CARTESIAN_POINT('Origin',(1.1,1.,32.5));
#10556=CARTESIAN_POINT('',(2.,1.,23.25));
#10557=CARTESIAN_POINT('',(1.2,1.,23.25));
#10558=CARTESIAN_POINT('Origin',(1.2,3.,14.));
#10559=CARTESIAN_POINT('',(1.2,3.,14.));
#10560=CARTESIAN_POINT('',(1.2,3.,14.));
#10561=CARTESIAN_POINT('',(1.2,-3.,14.));
#10562=CARTESIAN_POINT('',(1.2,3.,14.));
#10563=CARTESIAN_POINT('',(1.2,-3.,40.));
#10564=CARTESIAN_POINT('',(1.2,-3.,14.));
#10565=CARTESIAN_POINT('',(1.2,3.,40.));
#10566=CARTESIAN_POINT('',(1.2,3.,40.));
#10567=CARTESIAN_POINT('',(1.2,3.,14.));
#10568=CARTESIAN_POINT('Origin',(2.,3.,14.));
#10569=CARTESIAN_POINT('',(2.,3.,14.));
#10570=CARTESIAN_POINT('',(2.,3.,14.));
#10571=CARTESIAN_POINT('',(2.,3.,14.));
#10572=CARTESIAN_POINT('Origin',(2.,3.,14.));
#10573=CARTESIAN_POINT('',(2.,3.,40.));
#10574=CARTESIAN_POINT('',(2.,3.,40.));
#10575=CARTESIAN_POINT('',(2.,3.,14.));
#10576=CARTESIAN_POINT('Origin',(2.,-3.,14.));
#10577=CARTESIAN_POINT('',(2.,-3.,40.));
#10578=CARTESIAN_POINT('',(2.,-3.,40.));
#10579=CARTESIAN_POINT('',(2.,-3.,14.));
#10580=CARTESIAN_POINT('',(2.,-3.,14.));
#10581=CARTESIAN_POINT('',(2.,-3.,14.));
#10582=CARTESIAN_POINT('Origin',(1.2,-3.,14.));
#10583=CARTESIAN_POINT('',(1.2,-3.,14.));
#10584=CARTESIAN_POINT('',(1.2,-3.,40.));
#10585=CARTESIAN_POINT('Origin',(1.6,0.,40.));
#10586=CARTESIAN_POINT('Origin',(1.6,0.,14.));
#10587=CARTESIAN_POINT('',(0.,0.,0.));
#10588=CARTESIAN_POINT('Origin',(-1.5,2.,15.55));
#10589=CARTESIAN_POINT('',(-1.4,2.,15.825));
#10590=CARTESIAN_POINT('Origin',(-1.4,2.,15.55));
#10591=CARTESIAN_POINT('',(1.2,2.,15.825));
#10592=CARTESIAN_POINT('',(-1.5,2.,15.825));
#10593=CARTESIAN_POINT('Origin',(1.2,2.,15.55));
#10594=CARTESIAN_POINT('Origin',(1.2,2.8,15.1));
#10595=CARTESIAN_POINT('',(1.2,2.8,15.1));
#10596=CARTESIAN_POINT('',(-1.4,2.8,15.1));
#10597=CARTESIAN_POINT('',(1.2,2.8,15.1));
#10598=CARTESIAN_POINT('',(-1.4,2.8,16.));
#10599=CARTESIAN_POINT('',(-1.4,2.8,15.1));
#10600=CARTESIAN_POINT('',(1.2,2.8,16.));
#10601=CARTESIAN_POINT('',(1.2,2.8,16.));
#10602=CARTESIAN_POINT('',(1.2,2.8,15.1));
#10603=CARTESIAN_POINT('Origin',(1.2,1.2,15.1));
#10604=CARTESIAN_POINT('',(1.2,1.2,15.1));
#10605=CARTESIAN_POINT('',(1.2,1.2,15.1));
#10606=CARTESIAN_POINT('',(1.2,1.2,16.));
#10607=CARTESIAN_POINT('',(1.2,1.2,16.));
#10608=CARTESIAN_POINT('',(1.2,1.2,15.1));
#10609=CARTESIAN_POINT('Origin',(-1.4,1.2,15.1));
#10610=CARTESIAN_POINT('',(-1.4,1.2,15.1));
#10611=CARTESIAN_POINT('',(-1.4,1.2,15.1));
#10612=CARTESIAN_POINT('',(-1.4,1.2,16.));
#10613=CARTESIAN_POINT('',(-1.4,1.2,16.));
#10614=CARTESIAN_POINT('',(-1.4,1.2,15.1));
#10615=CARTESIAN_POINT('Origin',(-1.4,2.8,15.1));
#10616=CARTESIAN_POINT('',(-1.4,2.8,15.1));
#10617=CARTESIAN_POINT('',(-1.4,2.8,16.));
#10618=CARTESIAN_POINT('Origin',(-0.1,2.,16.));
#10619=CARTESIAN_POINT('Origin',(-0.1,2.,15.1));
#10620=CARTESIAN_POINT('',(0.,0.,0.));
#10621=CARTESIAN_POINT('Origin',(-1.5,2.,33.45));
#10622=CARTESIAN_POINT('',(-1.4,2.,33.725));
#10623=CARTESIAN_POINT('Origin',(-1.4,2.,33.45));
#10624=CARTESIAN_POINT('',(1.2,2.,33.725));
#10625=CARTESIAN_POINT('',(-1.5,2.,33.725));
#10626=CARTESIAN_POINT('Origin',(1.2,2.,33.45));
#10627=CARTESIAN_POINT('Origin',(1.2,2.8,33.));
#10628=CARTESIAN_POINT('',(1.2,2.8,33.));
#10629=CARTESIAN_POINT('',(-1.4,2.8,33.));
#10630=CARTESIAN_POINT('',(1.2,2.8,33.));
#10631=CARTESIAN_POINT('',(-1.4,2.8,33.9));
#10632=CARTESIAN_POINT('',(-1.4,2.8,33.));
#10633=CARTESIAN_POINT('',(1.2,2.8,33.9));
#10634=CARTESIAN_POINT('',(1.2,2.8,33.9));
#10635=CARTESIAN_POINT('',(1.2,2.8,33.));
#10636=CARTESIAN_POINT('Origin',(1.2,1.2,33.));
#10637=CARTESIAN_POINT('',(1.2,1.2,33.));
#10638=CARTESIAN_POINT('',(1.2,1.2,33.));
#10639=CARTESIAN_POINT('',(1.2,1.2,33.9));
#10640=CARTESIAN_POINT('',(1.2,1.2,33.9));
#10641=CARTESIAN_POINT('',(1.2,1.2,33.));
#10642=CARTESIAN_POINT('Origin',(-1.4,1.2,33.));
#10643=CARTESIAN_POINT('',(-1.4,1.2,33.));
#10644=CARTESIAN_POINT('',(-1.4,1.2,33.));
#10645=CARTESIAN_POINT('',(-1.4,1.2,33.9));
#10646=CARTESIAN_POINT('',(-1.4,1.2,33.9));
#10647=CARTESIAN_POINT('',(-1.4,1.2,33.));
#10648=CARTESIAN_POINT('Origin',(-1.4,2.8,33.));
#10649=CARTESIAN_POINT('',(-1.4,2.8,33.));
#10650=CARTESIAN_POINT('',(-1.4,2.8,33.9));
#10651=CARTESIAN_POINT('Origin',(-0.1,2.,33.9));
#10652=CARTESIAN_POINT('Origin',(-0.1,2.,33.));
#10653=CARTESIAN_POINT('',(0.,0.,0.));
#10654=CARTESIAN_POINT('Origin',(-5.2,0.,-0.1));
#10655=CARTESIAN_POINT('',(-5.425,-2.75545529808154E-17,0.));
#10656=CARTESIAN_POINT('Origin',(-5.2,0.,0.));
#10657=CARTESIAN_POINT('',(-5.425,2.75545529808154E-17,1.));
#10658=CARTESIAN_POINT('',(-5.425,-2.75545529808154E-17,-0.1));
#10659=CARTESIAN_POINT('Origin',(-5.2,0.,1.));
#10660=CARTESIAN_POINT('Origin',(-8.8,0.,-0.1));
#10661=CARTESIAN_POINT('',(-9.025,-2.75545529808154E-17,0.));
#10662=CARTESIAN_POINT('Origin',(-8.8,0.,0.));
#10663=CARTESIAN_POINT('',(-9.025,2.75545529808154E-17,1.));
#10664=CARTESIAN_POINT('',(-9.025,-2.75545529808154E-17,-0.1));
#10665=CARTESIAN_POINT('Origin',(-8.8,0.,1.));
#10666=CARTESIAN_POINT('Origin',(-7.,0.,1.));
#10667=CARTESIAN_POINT('',(-8.1,-1.34711147906209E-16,1.4));
#10668=CARTESIAN_POINT('Origin',(-7.,0.,1.4));
#10669=CARTESIAN_POINT('',(-8.1,-1.34711147906209E-16,1.));
#10670=CARTESIAN_POINT('',(-8.1,-1.34711147906209E-16,1.));
#10671=CARTESIAN_POINT('Origin',(-7.,0.,1.));
#10672=CARTESIAN_POINT('Origin',(-7.,0.,1.));
#10673=CARTESIAN_POINT('',(-8.5,-1.83697019872103E-16,1.4));
#10674=CARTESIAN_POINT('Origin',(-7.,0.,1.4));
#10675=CARTESIAN_POINT('',(-8.5,-1.83697019872103E-16,1.));
#10676=CARTESIAN_POINT('',(-8.5,-1.83697019872103E-16,1.));
#10677=CARTESIAN_POINT('Origin',(-7.,0.,1.));
#10678=CARTESIAN_POINT('Origin',(-7.,0.,1.4));
#10679=CARTESIAN_POINT('Origin',(-7.,0.,1.));
#10680=CARTESIAN_POINT('',(-9.2,-2.69422295812418E-16,1.));
#10681=CARTESIAN_POINT('Origin',(-7.,0.,1.));
#10682=CARTESIAN_POINT('Origin',(-7.,0.,0.));
#10683=CARTESIAN_POINT('',(-9.2,-2.69422295812418E-16,0.));
#10684=CARTESIAN_POINT('',(-9.2,-2.69422295812418E-16,0.));
#10685=CARTESIAN_POINT('Origin',(-7.,0.,0.));
#10686=CARTESIAN_POINT('Origin',(-7.,0.,1.));
#10687=CARTESIAN_POINT('Origin',(-7.,0.,0.));
#10688=CARTESIAN_POINT('',(0.,0.,0.));
#10689=CARTESIAN_POINT('Origin',(-7.,0.,1.4));
#10690=CARTESIAN_POINT('',(-8.1,-1.34711147906209E-16,20.));
#10691=CARTESIAN_POINT('Origin',(-7.,0.,20.));
#10692=CARTESIAN_POINT('',(-8.1,-1.34711147906209E-16,1.4));
#10693=CARTESIAN_POINT('',(-8.1,-1.34711147906209E-16,1.4));
#10694=CARTESIAN_POINT('Origin',(-7.,0.,1.4));
#10695=CARTESIAN_POINT('Origin',(-7.,0.,1.4));
#10696=CARTESIAN_POINT('',(-8.3,-1.59204083889156E-16,20.));
#10697=CARTESIAN_POINT('Origin',(-7.,0.,20.));
#10698=CARTESIAN_POINT('',(-8.3,-1.59204083889156E-16,1.4));
#10699=CARTESIAN_POINT('',(-8.3,-1.59204083889156E-16,1.4));
#10700=CARTESIAN_POINT('Origin',(-7.,0.,1.4));
#10701=CARTESIAN_POINT('Origin',(-7.,0.,20.));
#10702=CARTESIAN_POINT('Origin',(-7.,0.,1.4));
#10703=CARTESIAN_POINT('',(0.,0.,0.));
#10704=CARTESIAN_POINT('Origin',(-5.2,0.,19.9));
#10705=CARTESIAN_POINT('',(-5.425,-2.75545529808154E-17,20.));
#10706=CARTESIAN_POINT('Origin',(-5.2,0.,20.));
#10707=CARTESIAN_POINT('',(-5.425,2.75545529808154E-17,20.8));
#10708=CARTESIAN_POINT('',(-5.425,-2.75545529808154E-17,19.9));
#10709=CARTESIAN_POINT('Origin',(-5.2,0.,20.8));
#10710=CARTESIAN_POINT('Origin',(-8.8,0.,19.9));
#10711=CARTESIAN_POINT('',(-9.025,-2.75545529808154E-17,20.));
#10712=CARTESIAN_POINT('Origin',(-8.8,0.,20.));
#10713=CARTESIAN_POINT('',(-9.025,2.75545529808154E-17,20.8));
#10714=CARTESIAN_POINT('',(-9.025,-2.75545529808154E-17,19.9));
#10715=CARTESIAN_POINT('Origin',(-8.8,0.,20.8));
#10716=CARTESIAN_POINT('Origin',(-7.,0.,20.5));
#10717=CARTESIAN_POINT('',(-8.01,-1.23689326713883E-16,20.5));
#10718=CARTESIAN_POINT('Origin',(-7.,0.,20.5));
#10719=CARTESIAN_POINT('',(-8.01,1.23689326713883E-16,20.8));
#10720=CARTESIAN_POINT('',(-8.01,-1.23689326713883E-16,20.5));
#10721=CARTESIAN_POINT('Origin',(-7.,0.,20.8));
#10722=CARTESIAN_POINT('Origin',(-7.,0.,20.5));
#10723=CARTESIAN_POINT('',(-7.605,-7.40911313484149E-17,20.5));
#10724=CARTESIAN_POINT('Origin',(-7.,0.,20.5));
#10725=CARTESIAN_POINT('Origin',(-7.,0.,19.4));
#10726=CARTESIAN_POINT('',(-8.09,-1.33486501107061E-16,20.));
#10727=CARTESIAN_POINT('Origin',(-7.,0.,20.));
#10728=CARTESIAN_POINT('',(-8.09,-1.33486501107061E-16,19.4));
#10729=CARTESIAN_POINT('',(-8.09,-1.33486501107061E-16,19.4));
#10730=CARTESIAN_POINT('Origin',(-7.,0.,19.4));
#10731=CARTESIAN_POINT('Origin',(-7.,0.,19.4));
#10732=CARTESIAN_POINT('',(-7.605,-7.40911313484149E-17,19.4));
#10733=CARTESIAN_POINT('Origin',(-7.,0.,19.4));
#10734=CARTESIAN_POINT('Origin',(-7.,0.,20.));
#10735=CARTESIAN_POINT('',(-7.605,-7.40911313484149E-17,20.));
#10736=CARTESIAN_POINT('Origin',(-7.,0.,20.));
#10737=CARTESIAN_POINT('',(-9.2,-2.69422295812418E-16,20.8));
#10738=CARTESIAN_POINT('Origin',(-7.,0.,20.8));
#10739=CARTESIAN_POINT('',(-9.2,-2.69422295812418E-16,20.));
#10740=CARTESIAN_POINT('',(-9.2,-2.69422295812418E-16,20.));
#10741=CARTESIAN_POINT('Origin',(-7.,0.,20.));
#10742=CARTESIAN_POINT('Origin',(-7.,0.,20.8));
#10743=CARTESIAN_POINT('Origin',(-7.,0.,20.));
#10744=CARTESIAN_POINT('',(0.,0.,0.));
#10745=CARTESIAN_POINT('Origin',(-8.8,0.,20.));
#10746=CARTESIAN_POINT('',(-9.1,-3.67394039744207E-17,20.));
#10747=CARTESIAN_POINT('Origin',(-8.8,0.,20.));
#10748=CARTESIAN_POINT('',(-9.,-2.4492935982947E-17,20.));
#10749=CARTESIAN_POINT('Origin',(-8.8,0.,20.));
#10750=CARTESIAN_POINT('Origin',(-8.8,0.,1.));
#10751=CARTESIAN_POINT('',(-9.1,-3.67394039744207E-17,1.));
#10752=CARTESIAN_POINT('Origin',(-8.8,0.,1.));
#10753=CARTESIAN_POINT('',(-9.,2.4492935982947E-17,1.));
#10754=CARTESIAN_POINT('Origin',(-8.8,0.,1.));
#10755=CARTESIAN_POINT('Origin',(-8.8,0.,1.));
#10756=CARTESIAN_POINT('',(-9.1,-3.67394039744207E-17,1.));
#10757=CARTESIAN_POINT('Origin',(-8.8,0.,-0.6));
#10758=CARTESIAN_POINT('',(-9.,-2.4492935982947E-17,-0.6));
#10759=CARTESIAN_POINT('',(-9.,-2.4492935982947E-17,-0.6));
#10760=CARTESIAN_POINT('Origin',(-8.8,0.,-0.6));
#10761=CARTESIAN_POINT('Origin',(-8.8,0.,-0.6));
#10762=CARTESIAN_POINT('',(-9.,-2.4492935982947E-17,21.6));
#10763=CARTESIAN_POINT('Origin',(-8.8,0.,21.6));
#10764=CARTESIAN_POINT('',(-9.,-2.4492935982947E-17,-0.6));
#10765=CARTESIAN_POINT('Origin',(-8.8,0.,21.6));
#10766=CARTESIAN_POINT('Origin',(-8.8,0.,-0.6));
#10767=CARTESIAN_POINT('',(0.,0.,0.));
#10768=CARTESIAN_POINT('Origin',(-8.8,0.,20.8));
#10769=CARTESIAN_POINT('',(-8.965,-2.02066721859312E-17,21.2));
#10770=CARTESIAN_POINT('Origin',(-8.8,0.,21.2));
#10771=CARTESIAN_POINT('',(-8.965,-2.02066721859312E-17,20.8));
#10772=CARTESIAN_POINT('',(-8.965,-2.02066721859312E-17,20.8));
#10773=CARTESIAN_POINT('Origin',(-8.8,0.,20.8));
#10774=CARTESIAN_POINT('Origin',(-8.8,0.,20.8));
#10775=CARTESIAN_POINT('',(-9.2,-4.89858719658942E-17,21.2));
#10776=CARTESIAN_POINT('Origin',(-8.8,0.,21.2));
#10777=CARTESIAN_POINT('',(-9.2,-4.89858719658942E-17,20.8));
#10778=CARTESIAN_POINT('',(-9.2,-4.89858719658942E-17,20.8));
#10779=CARTESIAN_POINT('Origin',(-8.8,0.,20.8));
#10780=CARTESIAN_POINT('Origin',(-8.8,0.,21.2));
#10781=CARTESIAN_POINT('Origin',(-8.8,0.,20.8));
#10782=CARTESIAN_POINT('',(0.,0.,0.));
#10783=CARTESIAN_POINT('Origin',(-5.2,0.,20.));
#10784=CARTESIAN_POINT('',(-5.5,-3.67394039744206E-17,20.));
#10785=CARTESIAN_POINT('Origin',(-5.2,0.,20.));
#10786=CARTESIAN_POINT('',(-5.4,-2.44929359829471E-17,20.));
#10787=CARTESIAN_POINT('Origin',(-5.2,0.,20.));
#10788=CARTESIAN_POINT('Origin',(-5.2,0.,1.));
#10789=CARTESIAN_POINT('',(-5.5,-3.67394039744206E-17,1.));
#10790=CARTESIAN_POINT('Origin',(-5.2,0.,1.));
#10791=CARTESIAN_POINT('',(-5.4,2.44929359829471E-17,1.));
#10792=CARTESIAN_POINT('Origin',(-5.2,0.,1.));
#10793=CARTESIAN_POINT('Origin',(-5.2,0.,1.));
#10794=CARTESIAN_POINT('',(-5.5,-3.67394039744206E-17,1.));
#10795=CARTESIAN_POINT('Origin',(-5.2,0.,-0.6));
#10796=CARTESIAN_POINT('',(-5.4,-2.44929359829471E-17,-0.6));
#10797=CARTESIAN_POINT('',(-5.4,-2.44929359829471E-17,-0.6));
#10798=CARTESIAN_POINT('Origin',(-5.2,0.,-0.6));
#10799=CARTESIAN_POINT('Origin',(-5.2,0.,-0.6));
#10800=CARTESIAN_POINT('',(-5.4,-2.44929359829471E-17,21.6));
#10801=CARTESIAN_POINT('Origin',(-5.2,0.,21.6));
#10802=CARTESIAN_POINT('',(-5.4,-2.44929359829471E-17,-0.6));
#10803=CARTESIAN_POINT('Origin',(-5.2,0.,21.6));
#10804=CARTESIAN_POINT('Origin',(-5.2,0.,-0.6));
#10805=CARTESIAN_POINT('',(0.,0.,0.));
#10806=CARTESIAN_POINT('Origin',(-5.2,0.,20.8));
#10807=CARTESIAN_POINT('',(-5.365,-2.02066721859313E-17,21.2));
#10808=CARTESIAN_POINT('Origin',(-5.2,0.,21.2));
#10809=CARTESIAN_POINT('',(-5.365,-2.02066721859313E-17,20.8));
#10810=CARTESIAN_POINT('',(-5.365,-2.02066721859313E-17,20.8));
#10811=CARTESIAN_POINT('Origin',(-5.2,0.,20.8));
#10812=CARTESIAN_POINT('Origin',(-5.2,0.,20.8));
#10813=CARTESIAN_POINT('',(-5.6,-4.89858719658942E-17,21.2));
#10814=CARTESIAN_POINT('Origin',(-5.2,0.,21.2));
#10815=CARTESIAN_POINT('',(-5.6,-4.89858719658942E-17,20.8));
#10816=CARTESIAN_POINT('',(-5.6,-4.89858719658942E-17,20.8));
#10817=CARTESIAN_POINT('Origin',(-5.2,0.,20.8));
#10818=CARTESIAN_POINT('Origin',(-5.2,0.,21.2));
#10819=CARTESIAN_POINT('Origin',(-5.2,0.,20.8));
#10820=CARTESIAN_POINT('',(0.,0.,0.));
#10821=CARTESIAN_POINT('Ctrl Pts',(-6.20000025990999,0.00193246945643844,
1.00003735833913));
#10822=CARTESIAN_POINT('Ctrl Pts',(-6.20002044487095,0.15201065585541,1.00584212579936));
#10823=CARTESIAN_POINT('Ctrl Pts',(-6.28611355781982,0.450654413607575,
1.01745595262984));
#10824=CARTESIAN_POINT('Ctrl Pts',(-6.63487773043299,0.762776896374944,
1.0349026678303));
#10825=CARTESIAN_POINT('Ctrl Pts',(-7.09661480461016,0.841046944166038,
1.05237210147879));
#10826=CARTESIAN_POINT('Ctrl Pts',(-7.5301000809641,0.66191148032223,1.06986555847399));
#10827=CARTESIAN_POINT('Ctrl Pts',(-7.8019176387512,0.278705057923738,1.08738232429735));
#10828=CARTESIAN_POINT('Ctrl Pts',(-7.82838413701279,-0.19084760704926,
1.10492270302733));
#10829=CARTESIAN_POINT('Ctrl Pts',(-7.60064075566285,-0.603137091155931,
1.12248646715818));
#10830=CARTESIAN_POINT('Ctrl Pts',(-7.1879122444388,-0.831327694844811,
1.1400736154085));
#10831=CARTESIAN_POINT('Ctrl Pts',(-6.71648331627183,-0.804952825733149,
1.15768402928987));
#10832=CARTESIAN_POINT('Ctrl Pts',(-6.33069129380762,-0.53139586788873,
1.17531762920689));
#10833=CARTESIAN_POINT('Ctrl Pts',(-6.17986938434826,-0.166924530929506,
1.19003152205635));
#10834=CARTESIAN_POINT('Ctrl Pts',(-6.18891827393114,0.139694417819641,
1.20181411747366));
#10835=CARTESIAN_POINT('Ctrl Pts',(-6.28167759636603,0.432287479563812,
1.21360434390419));
#10836=CARTESIAN_POINT('Ctrl Pts',(-6.54498491257115,0.727352514001043,
1.22835639528026));
#10837=CARTESIAN_POINT('Ctrl Pts',(-7.00178799837524,0.858989074734809,
1.2460815491715));
#10838=CARTESIAN_POINT('Ctrl Pts',(-7.45905640505002,0.727341633611197,
1.2638292469814));
#10839=CARTESIAN_POINT('Ctrl Pts',(-7.77665281049733,0.372097321399229,
1.28159932797245));
#10840=CARTESIAN_POINT('Ctrl Pts',(-7.85663990835041,-0.0982374580424732,
1.29939162334549));
#10841=CARTESIAN_POINT('Ctrl Pts',(-7.67391806687674,-0.539592338752092,
1.31720595246947));
#10842=CARTESIAN_POINT('Ctrl Pts',(-7.28390423314539,-0.816419475206943,
1.33504212338853));
#10843=CARTESIAN_POINT('Ctrl Pts',(-6.80581165670056,-0.843349744908527,
1.35289993632842));
#10844=CARTESIAN_POINT('Ctrl Pts',(-6.38616737126169,-0.61151281975725,
1.37077917836497));
#10845=CARTESIAN_POINT('Ctrl Pts',(-6.15391471330266,-0.191448545046746,
1.38867962991899));
#10846=CARTESIAN_POINT('Ctrl Pts',(-6.18078031189829,0.288356063072798,
1.40660105660474));
#10847=CARTESIAN_POINT('Ctrl Pts',(-6.45912099114284,0.680780452257456,
1.42454321935777));
#10848=CARTESIAN_POINT('Ctrl Pts',(-6.90408886634936,0.865172061566579,
1.44250586618275));
#10849=CARTESIAN_POINT('Ctrl Pts',(-7.37948719351768,0.784486199243698,
1.46048873474343));
#10850=CARTESIAN_POINT('Ctrl Pts',(-7.73949168252554,0.462850086060547,
1.47849155669373));
#10851=CARTESIAN_POINT('Ctrl Pts',(-7.87332738631526,-0.0014557841833066,
1.49651404939771));
#10852=CARTESIAN_POINT('Ctrl Pts',(-7.73949699110486,-0.466462821459191,
1.51455592727214));
#10853=CARTESIAN_POINT('Ctrl Pts',(-7.43853082628792,-0.735208997602771,
1.52960672657187));
#10854=CARTESIAN_POINT('Ctrl Pts',(-7.13950426621928,-0.830029799823059,
1.5416567556677));
#10855=CARTESIAN_POINT('Ctrl Pts',(-6.82573429908325,-0.839341203501555,
1.55371299076107));
#10856=CARTESIAN_POINT('Ctrl Pts',(-6.46884268588545,-0.691631510671627,
1.56812451918729));
#10857=CARTESIAN_POINT('Ctrl Pts',(-6.19953260950331,-0.335836989319061,
1.58489796930832));
#10858=CARTESIAN_POINT('Ctrl Pts',(-6.13558329245919,0.087838843174565,
1.60101457637617));
#10859=CARTESIAN_POINT('Ctrl Pts',(-6.28224419701691,0.490989051876738,
1.61714503893002));
#10860=CARTESIAN_POINT('Ctrl Pts',(-6.60413478737033,0.775061465279082,
1.63328911262099));
#10861=CARTESIAN_POINT('Ctrl Pts',(-7.02294084448011,0.870730250827747,
1.64944654818199));
#10862=CARTESIAN_POINT('Ctrl Pts',(-7.43707348216018,0.754258049077075,
1.66561709103637));
#10863=CARTESIAN_POINT('Ctrl Pts',(-7.74477169774561,0.453838654047166,
1.68180048156974));
#10864=CARTESIAN_POINT('Ctrl Pts',(-7.88680288613318,-0.003482702933719,
1.69979600813884));
#10865=CARTESIAN_POINT('Ctrl Pts',(-7.73694295256561,-0.521688074393446,
1.71960864643413));
#10866=CARTESIAN_POINT('Ctrl Pts',(-7.2579246797109,-0.866176668338957,
1.74124367709995));
#10867=CARTESIAN_POINT('Ctrl Pts',(-6.71798257071652,-0.843361624137061,
1.76109465157299));
#10868=CARTESIAN_POINT('Ctrl Pts',(-6.32813840204838,-0.562067108424238,
1.779155502939));
#10869=CARTESIAN_POINT('Ctrl Pts',(-6.1403602470473,-0.172779460138823,
1.79542117132473));
#10870=CARTESIAN_POINT('Ctrl Pts',(-6.16191594592092,0.259681676239064,
1.81169744765855));
#10871=CARTESIAN_POINT('Ctrl Pts',(-6.38773509477738,0.629211178523826,
1.82798403284572));
#10872=CARTESIAN_POINT('Ctrl Pts',(-6.76298297690006,0.845905336791279,
1.84428062449289));
#10873=CARTESIAN_POINT('Ctrl Pts',(-7.1966047520639,0.856877177797125,1.86058691436274));
#10874=CARTESIAN_POINT('Ctrl Pts',(-7.51813159987616,0.691704323104765,
1.87418331464002));
#10875=CARTESIAN_POINT('Ctrl Pts',(-7.70496340534196,0.479537214773933,
1.88506497141452));
#10876=CARTESIAN_POINT('Ctrl Pts',(-7.834243376472,0.228058843588403,1.89594960161061));
#10877=CARTESIAN_POINT('Ctrl Pts',(-7.87040214071621,-0.132058080538115,
1.90956086256863));
#10878=CARTESIAN_POINT('Ctrl Pts',(-7.70176729712619,-0.532544739489079,
1.92590281458038));
#10879=CARTESIAN_POINT('Ctrl Pts',(-7.3617541753632,-0.803795766305812,
1.94225288140178));
#10880=CARTESIAN_POINT('Ctrl Pts',(-6.96910081682361,-0.872691342258758,
1.95724758038991));
#10881=CARTESIAN_POINT('Ctrl Pts',(-6.62358365553027,-0.779878922686934,
1.97088456464667));
#10882=CARTESIAN_POINT('Ctrl Pts',(-6.36438571820951,-0.588772954661729,
1.98316190508021));
#10883=CARTESIAN_POINT('Ctrl Pts',(-6.19306544459119,-0.315928048614165,
1.99544316011942));
#10884=CARTESIAN_POINT('Ctrl Pts',(-6.13303928680132,0.000731296674565001,
2.00772818860116));
#10885=CARTESIAN_POINT('Ctrl Pts',(-6.19306246181983,0.31737131710264,2.02001684693935));
#10886=CARTESIAN_POINT('Ctrl Pts',(-6.36452596264878,0.590662777058206,
2.03230899246722));
#10887=CARTESIAN_POINT('Ctrl Pts',(-6.62407285476001,0.781608449704824,
2.04460448181281));
#10888=CARTESIAN_POINT('Ctrl Pts',(-7.03960726862712,0.894452101215339,
2.06100273047082));
#10889=CARTESIAN_POINT('Ctrl Pts',(-7.58098213708746,0.728278840923384,
2.08150817561209));
#10890=CARTESIAN_POINT('Ctrl Pts',(-7.9216670182819,0.138324035331395,2.10612575173056));
#10891=CARTESIAN_POINT('Ctrl Pts',(-7.77006105183817,-0.525438678362505,
2.13075319116009));
#10892=CARTESIAN_POINT('Ctrl Pts',(-7.20723620509449,-0.909325593088126,
2.15538930422495));
#10893=CARTESIAN_POINT('Ctrl Pts',(-6.53333888373858,-0.807749099412924,
2.18003289797092));
#10894=CARTESIAN_POINT('Ctrl Pts',(-6.1083188432114,-0.274839326778277,
2.204682767912));
#10895=CARTESIAN_POINT('Ctrl Pts',(-6.15924265883207,0.405062095085805,
2.22933770998693));
#10896=CARTESIAN_POINT('Ctrl Pts',(-6.65910391363797,0.868885188693027,
2.25399651054932));
#10897=CARTESIAN_POINT('Ctrl Pts',(-7.34108037988483,0.868897827671466,
2.2786579570982));
#10898=CARTESIAN_POINT('Ctrl Pts',(-7.84103724749041,0.405011680967366,
2.30332083156262));
#10899=CARTESIAN_POINT('Ctrl Pts',(-7.89200269882987,-0.275103355231245,
2.32798391722886));
#10900=CARTESIAN_POINT('Ctrl Pts',(-7.46677961363602,-0.808302976870588,
2.35264599503351));
#10901=CARTESIAN_POINT('Ctrl Pts',(-6.79246102077101,-0.909925026569516,
2.37730584883283));
#10902=CARTESIAN_POINT('Ctrl Pts',(-6.22911235514946,-0.525814889228737,
2.40196226239673));
#10903=CARTESIAN_POINT('Ctrl Pts',(-6.07744456821118,0.138809074175696,
2.42661402385257));
#10904=CARTESIAN_POINT('Ctrl Pts',(-6.41824880300263,0.729027866722014,
2.45125992491537));
#10905=CARTESIAN_POINT('Ctrl Pts',(-7.06934122876124,0.929824149026898,
2.47589876067858));
#10906=CARTESIAN_POINT('Ctrl Pts',(-7.68299796183915,0.634246527935802,
2.50052933613646));
#10907=CARTESIAN_POINT('Ctrl Pts',(-7.93168967879738,0.000445263131447748,
2.52515045678013));
#10908=CARTESIAN_POINT('Ctrl Pts',(-7.68302213647328,-0.633094458923734,
2.54976094441856));
#10909=CARTESIAN_POINT('Ctrl Pts',(-7.07007700890629,-0.928102101680422,
2.57435962067245));
#10910=CARTESIAN_POINT('Ctrl Pts',(-6.42054771123064,-0.727833461900544,
2.59894532553828));
#10911=CARTESIAN_POINT('Ctrl Pts',(-6.08063030273252,-0.138905152375385,
2.62351690334527));
#10912=CARTESIAN_POINT('Ctrl Pts',(-6.20716604633801,0.411896009844242,
2.64398049630671));
#10913=CARTESIAN_POINT('Ctrl Pts',(-6.51199774209192,0.714676452673333,
2.66034317170459));
#10914=CARTESIAN_POINT('Ctrl Pts',(-6.80647130896726,0.843685013671235,
2.67261094147259));
#10915=CARTESIAN_POINT('Ctrl Pts',(-7.12812476587158,0.855502087711664,
2.68487433317324));
#10916=CARTESIAN_POINT('Ctrl Pts',(-7.43161948042588,0.749419002627999,
2.69713320958533));
#10917=CARTESIAN_POINT('Ctrl Pts',(-7.67521904640705,0.539636596661724,
2.7093874343511));
#10918=CARTESIAN_POINT('Ctrl Pts',(-7.82547325176268,0.255576344693996,
2.72163687040038));
#10919=CARTESIAN_POINT('Ctrl Pts',(-7.86123160253771,-0.0635635909156293,
2.73388138286896));
#10920=CARTESIAN_POINT('Ctrl Pts',(-7.76460027897753,-0.425533717492343,
2.74816074914963));
#10921=CARTESIAN_POINT('Ctrl Pts',(-7.47374360660769,-0.751894656156828,
2.76447137187111));
#10922=CARTESIAN_POINT('Ctrl Pts',(-7.00091436223893,-0.88782428734477,
2.78280870439184));
#10923=CARTESIAN_POINT('Ctrl Pts',(-6.52888862282209,-0.751805319722163,
2.80113347394993));
#10924=CARTESIAN_POINT('Ctrl Pts',(-6.2016684053735,-0.385612928895403,
2.81944525307317));
#10925=CARTESIAN_POINT('Ctrl Pts',(-6.11955382035284,0.0981170754742554,
2.83774361225262));
#10926=CARTESIAN_POINT('Ctrl Pts',(-6.30722625617569,0.551073055321834,
2.85602813457377));
#10927=CARTESIAN_POINT('Ctrl Pts',(-6.70680747045044,0.834525970819447,
2.87429840546262));
#10928=CARTESIAN_POINT('Ctrl Pts',(-7.19559869716282,0.861909407171868,
2.8925540164347));
#10929=CARTESIAN_POINT('Ctrl Pts',(-7.62360216624703,0.625277985438662,
2.91079457296321));
#10930=CARTESIAN_POINT('Ctrl Pts',(-7.86012925287909,0.197486531354187,
2.92901967711976));
#10931=CARTESIAN_POINT('Ctrl Pts',(-7.83237012712838,-0.289941720567784,
2.94722894753945));
#10932=CARTESIAN_POINT('Ctrl Pts',(-7.55008001741224,-0.687784692046307,
2.96542200407487));
#10933=CARTESIAN_POINT('Ctrl Pts',(-7.09977586824996,-0.874247976731781,
2.98359847915852));
#10934=CARTESIAN_POINT('Ctrl Pts',(-6.61974323779859,-0.792623075615972,
3.00175800933));
#10935=CARTESIAN_POINT('Ctrl Pts',(-6.257058130519,-0.468413543112272,3.0199002388146));
#10936=CARTESIAN_POINT('Ctrl Pts',(-6.12258713457564,-0.00138700255432796,
3.03802482606703));
#10937=CARTESIAN_POINT('Ctrl Pts',(-6.25706727378645,0.465139317147603,
3.05613142853581));
#10938=CARTESIAN_POINT('Ctrl Pts',(-6.61877666867083,0.788285032559405,
3.07421972093098));
#10939=CARTESIAN_POINT('Ctrl Pts',(-7.09647607914372,0.869376408975484,
3.09228937996591));
#10940=CARTESIAN_POINT('Ctrl Pts',(-7.54362920385282,0.68408153123717,3.11034009649877));
#10941=CARTESIAN_POINT('Ctrl Pts',(-7.82336210739947,0.28970919078182,3.12837156650594));
#10942=CARTESIAN_POINT('Ctrl Pts',(-7.85036951729978,-0.192518648808231,
3.1463834953635));
#10943=CARTESIAN_POINT('Ctrl Pts',(-7.61693284376151,-0.614735291409423,
3.16437560200786));
#10944=CARTESIAN_POINT('Ctrl Pts',(-7.19511476226595,-0.847778676228102,
3.18234760781168));
#10945=CARTESIAN_POINT('Ctrl Pts',(-6.7145098999882,-0.820710857786535,
3.20029925009486));
#10946=CARTESIAN_POINT('Ctrl Pts',(-6.32242256217712,-0.542413764760527,
3.21823027098919));
#10947=CARTESIAN_POINT('Ctrl Pts',(-6.13871066850024,-0.098686345015634,
3.23614042632575));
#10948=CARTESIAN_POINT('Ctrl Pts',(-6.21914065946509,0.374211025419683,
3.25402947870679));
#10949=CARTESIAN_POINT('Ctrl Pts',(-6.53845875539302,0.731406338297415,
3.27189720144838));
#10950=CARTESIAN_POINT('Ctrl Pts',(-6.99831755296742,0.863804065639348,
3.2897433804432));
#10951=CARTESIAN_POINT('Ctrl Pts',(-7.45757029965599,0.731409466469204,
3.30756780748229));
#10952=CARTESIAN_POINT('Ctrl Pts',(-7.77559982146972,0.37540881511312,3.32537028850097));
#10953=CARTESIAN_POINT('Ctrl Pts',(-7.85537931424834,-0.094642652826617,
3.34315063708933));
#10954=CARTESIAN_POINT('Ctrl Pts',(-7.67307624395954,-0.534539169893111,
3.36090867961867));
#10955=CARTESIAN_POINT('Ctrl Pts',(-7.28516805861167,-0.809670332991083,
3.37864425091963));
#10956=CARTESIAN_POINT('Ctrl Pts',(-6.81094328129299,-0.836216654728318,
3.39635719733567));
#10957=CARTESIAN_POINT('Ctrl Pts',(-6.39581795219668,-0.606687244699812,
3.41404737686194));
#10958=CARTESIAN_POINT('Ctrl Pts',(-6.16673282986248,-0.192016386472062,
3.43171465630725));
#10959=CARTESIAN_POINT('Ctrl Pts',(-6.19335105955753,0.280356102113162,
3.44935891493111));
#10960=CARTESIAN_POINT('Ctrl Pts',(-6.46683379484748,0.665660108445628,
3.46698004190314));
#10961=CARTESIAN_POINT('Ctrl Pts',(-6.90284795213186,0.846152102600437,
3.48457793824716));
#10962=CARTESIAN_POINT('Ctrl Pts',(-7.36737219772646,0.767129205800447,
3.50215251490095));
#10963=CARTESIAN_POINT('Ctrl Pts',(-7.71834143496065,0.453434200086869,
3.51970369457236));
#10964=CARTESIAN_POINT('Ctrl Pts',(-7.82645846631761,0.077080609195679,
3.53431012488451));
#10965=CARTESIAN_POINT('Ctrl Pts',(-7.78351602643939,-0.223766099777631,
3.54598350983127));
#10966=CARTESIAN_POINT('Ctrl Pts',(-7.65984666406284,-0.501195016191524,
3.55764904771478));
#10967=CARTESIAN_POINT('Ctrl Pts',(-7.36883520137935,-0.761421141511966,
3.57221624328425));
#10968=CARTESIAN_POINT('Ctrl Pts',(-6.90699782821215,-0.839986918687281,
3.58967328199228));
#10969=CARTESIAN_POINT('Ctrl Pts',(-6.5235772119384,-0.680444831465126,
3.60516965595896));
#10970=CARTESIAN_POINT('Ctrl Pts',(-6.29205860881578,-0.410854643842501,
3.6187136684483));
#10971=CARTESIAN_POINT('Ctrl Pts',(-6.19144251696091,-0.123792268925567,
3.63031232027941));
#10972=CARTESIAN_POINT('Ctrl Pts',(-6.20295651325157,0.179997595512823,
3.64190047202365));
#10973=CARTESIAN_POINT('Ctrl Pts',(-6.32432621115477,0.458374743512086,
3.65347812777622));
#10974=CARTESIAN_POINT('Ctrl Pts',(-6.53898438351643,0.672840241042802,
3.66504529364933));
#10975=CARTESIAN_POINT('Ctrl Pts',(-6.81680637706894,0.794134031701534,
3.67660197812095));
#10976=CARTESIAN_POINT('Ctrl Pts',(-7.11950248291682,0.805397533837699,
3.68814819174188));
#10977=CARTESIAN_POINT('Ctrl Pts',(-7.34163561569263,0.727628486768507,
3.69712044609008));
#10978=CARTESIAN_POINT('Ctrl Pts',(-7.53458281141515,0.599570945127131,
3.70608728556614));
#10979=CARTESIAN_POINT('Ctrl Pts',(-7.71503532521363,0.400461841999,3.71632891696956));
#10980=CARTESIAN_POINT('Ctrl Pts',(-7.82528743114405,0.0430926937144543,
3.73039630239659));
#10981=CARTESIAN_POINT('Ctrl Pts',(-7.74111169379658,-0.37323537543407,
3.74636272256909));
#10982=CARTESIAN_POINT('Ctrl Pts',(-7.44499573228645,-0.704767123835098,
3.76294659713056));
#10983=CARTESIAN_POINT('Ctrl Pts',(-7.00172600054551,-0.832350159693755,
3.78014508956006));
#10984=CARTESIAN_POINT('Ctrl Pts',(-6.55926311085665,-0.704755991680177,
3.79732045846001));
#10985=CARTESIAN_POINT('Ctrl Pts',(-6.2528315275211,-0.361772892660608,
3.81447281592693));
#10986=CARTESIAN_POINT('Ctrl Pts',(-6.17601189131465,0.0911409447444953,
3.83160228337755));
#10987=CARTESIAN_POINT('Ctrl Pts',(-6.35159897954253,0.514776986788965,
3.84870899394101));
#10988=CARTESIAN_POINT('Ctrl Pts',(-6.72535286944806,0.780122083208515,
3.86579309179979));
#10989=CARTESIAN_POINT('Ctrl Pts',(-7.13122870473182,0.802254155922275,
3.88095899359145));
#10990=CARTESIAN_POINT('Ctrl Pts',(-7.44985202071078,0.662844517922881,
3.89421470788503));
#10991=CARTESIAN_POINT('Ctrl Pts',(-7.66049480984587,0.452421922662202,
3.90556689264628));
#10992=CARTESIAN_POINT('Ctrl Pts',(-7.77936222711058,0.179641079514188,
3.91690927461427));
#10993=CARTESIAN_POINT('Ctrl Pts',(-7.79055864897702,-0.117447939280878,
3.92824190893221));
#10994=CARTESIAN_POINT('Ctrl Pts',(-7.69235883457516,-0.397692735498425,
3.93956485365948));
#10995=CARTESIAN_POINT('Ctrl Pts',(-7.4988193112063,-0.622862064421365,
3.95087816922642));
#10996=CARTESIAN_POINT('Ctrl Pts',(-7.23669309425985,-0.760857052520071,
3.96218191668704));
#10997=CARTESIAN_POINT('Ctrl Pts',(-6.84397122474983,-0.806385392143749,
3.97724090685452));
#10998=CARTESIAN_POINT('Ctrl Pts',(-6.3759149329141,-0.581575494059258,
3.99604104936904));
#10999=CARTESIAN_POINT('Ctrl Pts',(-6.14801487092373,-0.00140577011587543,
4.01856401164168));
#11000=CARTESIAN_POINT('Ctrl Pts',(-6.37569406553146,0.577216837917985,
4.04105035155356));
#11001=CARTESIAN_POINT('Ctrl Pts',(-6.93503804704956,0.846504117962824,
4.06350067666592));
#11002=CARTESIAN_POINT('Ctrl Pts',(-7.52735353249786,0.663517124905538,
4.08591563261074));
#11003=CARTESIAN_POINT('Ctrl Pts',(-7.83667549320556,0.127633503183688,
4.10829588960443));
#11004=CARTESIAN_POINT('Ctrl Pts',(-7.69892862810743,-0.475216209100622,
4.13064214875721));
#11005=CARTESIAN_POINT('Ctrl Pts',(-7.24587822138796,-0.783213519985818,
4.15047591997482));
#11006=CARTESIAN_POINT('Ctrl Pts',(-6.78448909503242,-0.770150049272615,
4.16780939837816));
#11007=CARTESIAN_POINT('Ctrl Pts',(-6.44291255401028,-0.573358437418835,
4.18265244830762));
#11008=CARTESIAN_POINT('Ctrl Pts',(-6.23727444607057,-0.236582538920206,
4.19748151807985));
#11009=CARTESIAN_POINT('Ctrl Pts',(-6.21750233201011,0.156779347523281,
4.21229685032696));
#11010=CARTESIAN_POINT('Ctrl Pts',(-6.38851989967645,0.511421035774412,
4.22709868951428));
#11011=CARTESIAN_POINT('Ctrl Pts',(-6.68127276436824,0.721655369840554,
4.24065490665371));
#11012=CARTESIAN_POINT('Ctrl Pts',(-6.99873870462004,0.781500222137114,
4.25296927229394));
#11013=CARTESIAN_POINT('Ctrl Pts',(-7.28423799128053,0.727580241858167,
4.26404501085876));
#11014=CARTESIAN_POINT('Ctrl Pts',(-7.52996735384668,0.573044604556925,
4.27511366794562));
#11015=CARTESIAN_POINT('Ctrl Pts',(-7.70249233600175,0.339504000304913,
4.28617535676904));
#11016=CARTESIAN_POINT('Ctrl Pts',(-7.77704029199075,0.0596812865399207,
4.29723019232866));
#11017=CARTESIAN_POINT('Ctrl Pts',(-7.73493077249201,-0.32516426809182,
4.31196099263524));
#11018=CARTESIAN_POINT('Ctrl Pts',(-7.48195320169677,-0.642258532616097,
4.32667855077855));
#11019=CARTESIAN_POINT('Ctrl Pts',(-7.11676447072565,-0.768672906025829,
4.34138335007881));
#11020=CARTESIAN_POINT('Ctrl Pts',(-6.82822052968084,-0.75826459078673,
4.35240569057047));
#11021=CARTESIAN_POINT('Ctrl Pts',(-6.56324655367934,-0.642480501470498,
4.36342189483669));
#11022=CARTESIAN_POINT('Ctrl Pts',(-6.3590246126422,-0.438361948172784,
4.37443208856579));
#11023=CARTESIAN_POINT('Ctrl Pts',(-6.24366823031993,-0.173725992278803,
4.38543639651659));
#11024=CARTESIAN_POINT('Ctrl Pts',(-6.23278862096309,0.114603786226641,
4.39643494391794));
#11025=CARTESIAN_POINT('Ctrl Pts',(-6.32818140570146,0.3866727001158,4.40742785948479));
#11026=CARTESIAN_POINT('Ctrl Pts',(-6.54732728408833,0.641795528726263,
4.42024651101618));
#11027=CARTESIAN_POINT('Ctrl Pts',(-6.90966296029133,0.792450205988824,
4.43488744119146));
#11028=CARTESIAN_POINT('Ctrl Pts',(-7.34497884959273,0.718229352606656,
4.45134684847234));
#11029=CARTESIAN_POINT('Ctrl Pts',(-7.67373744220819,0.42439860304808,4.46779506017063));
#11030=CARTESIAN_POINT('Ctrl Pts',(-7.7957623026863,0.000795392209376382,
4.48423253597012));
#11031=CARTESIAN_POINT('Ctrl Pts',(-7.6737681501059,-0.422451523433032,
4.50065973137187));
#11032=CARTESIAN_POINT('Ctrl Pts',(-7.34550270887416,-0.715780174479536,
4.51707711746896));
#11033=CARTESIAN_POINT('Ctrl Pts',(-6.91173568096419,-0.789442989854855,
4.53348515869499));
#11034=CARTESIAN_POINT('Ctrl Pts',(-6.50548543634235,-0.62113576023861,
4.54988433137086));
#11035=CARTESIAN_POINT('Ctrl Pts',(-6.25117725190974,-0.26266942709969,
4.56627511486019));
#11036=CARTESIAN_POINT('Ctrl Pts',(-6.22657268391725,0.175941615799059,
4.58265798957595));
#11037=CARTESIAN_POINT('Ctrl Pts',(-6.43900037753832,0.560237327905976,
4.59903344336352));
#11038=CARTESIAN_POINT('Ctrl Pts',(-6.82315231070266,0.772532064615231,
4.61540196293227));
#11039=CARTESIAN_POINT('Ctrl Pts',(-7.2612181287951,0.747894614274433,4.63176404577646));
#11040=CARTESIAN_POINT('Ctrl Pts',(-7.61885424416052,0.494109349486934,
4.64812018315545));
#11041=CARTESIAN_POINT('Ctrl Pts',(-7.78669901230814,0.0889725746862699,
4.66447087596232));
#11042=CARTESIAN_POINT('Ctrl Pts',(-7.72532501848925,-0.270994143806812,
4.67809233336064));
#11043=CARTESIAN_POINT('Ctrl Pts',(-7.56738721688822,-0.506594326857297,
4.68898728035258));
#11044=CARTESIAN_POINT('Ctrl Pts',(-7.35097564028756,-0.689891456361417,
4.69988083117445));
#11045=CARTESIAN_POINT('Ctrl Pts',(-7.0003169174225,-0.79110738140522,4.71349530909451));
#11046=CARTESIAN_POINT('Ctrl Pts',(-6.57937611771461,-0.669773743535281,
4.72982925479887));
#11047=CARTESIAN_POINT('Ctrl Pts',(-6.28761734218788,-0.343284450620702,
4.74616028288309));
#11048=CARTESIAN_POINT('Ctrl Pts',(-6.21426971041073,0.0883871334668474,
4.76248890194073));
#11049=CARTESIAN_POINT('Ctrl Pts',(-6.38182100128212,0.492840639406237,
4.77881561989744));
#11050=CARTESIAN_POINT('Ctrl Pts',(-6.73884045313308,0.746153973023737,
4.79514095601288));
#11051=CARTESIAN_POINT('Ctrl Pts',(-7.17589338359863,0.770679755263529,
4.81146540426486));
#11052=CARTESIAN_POINT('Ctrl Pts',(-7.55900114520461,0.55894423669953,4.82778951061359));
#11053=CARTESIAN_POINT('Ctrl Pts',(-7.77075750409873,0.175788412965931,
4.84411370102291));
#11054=CARTESIAN_POINT('Ctrl Pts',(-7.74620736592161,-0.261233995076225,
4.86043866853608));
#11055=CARTESIAN_POINT('Ctrl Pts',(-7.49294321470503,-0.618448872812403,
4.87676449790797));
#11056=CARTESIAN_POINT('Ctrl Pts',(-7.08837163954946,-0.785730122461179,
4.89309260172666));
#11057=CARTESIAN_POINT('Ctrl Pts',(-6.65674407499508,-0.712671607108413,
4.90942182102584));
#11058=CARTESIAN_POINT('Ctrl Pts',(-6.33017289353631,-0.420518596063947,
4.92575590410514));
#11059=CARTESIAN_POINT('Ctrl Pts',(-6.2493887150478,-0.140566474730618,
4.93664355063335));
#11060=CARTESIAN_POINT('Ctrl Pts',(-6.24936976727053,0.000312488344807942,
4.94209250793942));
#11061=CARTESIAN_POINT('Ctrl Pts',(-6.21496022479178,0.00193045739649654,
1.00003735833913));
#11062=CARTESIAN_POINT('Ctrl Pts',(-6.21498003690632,0.149236475283263,
1.0057349030646));
#11063=CARTESIAN_POINT('Ctrl Pts',(-6.29946146307499,0.442287265692152,
1.01713084057243));
#11064=CARTESIAN_POINT('Ctrl Pts',(-6.64173420840598,0.74861847420515,1.03425315186381));
#11065=CARTESIAN_POINT('Ctrl Pts',(-7.09490182459049,0.825432047669671,
1.05139783360786));
#11066=CARTESIAN_POINT('Ctrl Pts',(-7.52036826388768,0.649617795679984,
1.06856728953495));
#11067=CARTESIAN_POINT('Ctrl Pts',(-7.7871742517923,0.273479603576055,1.08576001517786));
#11068=CARTESIAN_POINT('Ctrl Pts',(-7.81315997530967,-0.187447249693266,
1.10297754661545));
#11069=CARTESIAN_POINT('Ctrl Pts',(-7.589586767382,-0.592199963068705,1.12021926119168));
#11070=CARTESIAN_POINT('Ctrl Pts',(-7.18437407174804,-0.816243588302344,
1.13748556186172));
#11071=CARTESIAN_POINT('Ctrl Pts',(-6.72148059457952,-0.790355142963932,
1.15477626219657));
#11072=CARTESIAN_POINT('Ctrl Pts',(-6.34262910012066,-0.52172948451145,
1.17209170042211));
#11073=CARTESIAN_POINT('Ctrl Pts',(-6.19449971679954,-0.163784023548138,
1.18654139527825));
#11074=CARTESIAN_POINT('Ctrl Pts',(-6.2033859162291,0.137380889459928,1.19811412071467));
#11075=CARTESIAN_POINT('Ctrl Pts',(-6.29449904481813,0.424787607736377,
1.20969506869488));
#11076=CARTESIAN_POINT('Ctrl Pts',(-6.55315191262231,0.714650845840973,
1.22418580731435));
#11077=CARTESIAN_POINT('Ctrl Pts',(-7.0019550394566,0.843993903272686,1.24159980818703));
#11078=CARTESIAN_POINT('Ctrl Pts',(-7.45128651383865,0.714642167033589,
1.25903832129017));
#11079=CARTESIAN_POINT('Ctrl Pts',(-7.76342536249333,0.365519355718316,
1.27650157939527));
#11080=CARTESIAN_POINT('Ctrl Pts',(-7.84206012434238,-0.0967940191462743,
1.29398943844924));
#11081=CARTESIAN_POINT('Ctrl Pts',(-7.66243479502456,-0.530701874726786,
1.311501908922));
#11082=CARTESIAN_POINT('Ctrl Pts',(-7.27894550868061,-0.802913947461582,
1.3290389166792));
#11083=CARTESIAN_POINT('Ctrl Pts',(-6.80875585148875,-0.829412645711587,
1.34660041024838));
#11084=CARTESIAN_POINT('Ctrl Pts',(-6.39596178700798,-0.601376268456168,
1.3641863119731));
#11085=CARTESIAN_POINT('Ctrl Pts',(-6.16744602527253,-0.18810074316643,
1.38179653848221));
#11086=CARTESIAN_POINT('Ctrl Pts',(-6.19386832849657,0.284055727066803,
1.39943099486938));
#11087=CARTESIAN_POINT('Ctrl Pts',(-6.46781735673514,0.670315409844122,
1.41708956636422));
#11088=CARTESIAN_POINT('Ctrl Pts',(-6.905874703008,0.851860949298453,1.43477214942586));
#11089=CARTESIAN_POINT('Ctrl Pts',(-7.37400527438391,0.772425993272578,
1.45247857106921));
#11090=CARTESIAN_POINT('Ctrl Pts',(-7.72859756382396,0.455648564419921,
1.47020877245192));
#11091=CARTESIAN_POINT('Ctrl Pts',(-7.86046618774004,-0.00176530696331421,
1.4879623972667));
#11092=CARTESIAN_POINT('Ctrl Pts',(-7.72860440581187,-0.459992961560558,
1.50573970438362));
#11093=CARTESIAN_POINT('Ctrl Pts',(-7.43196756428821,-0.724892207153614,
1.52057285972636));
#11094=CARTESIAN_POINT('Ctrl Pts',(-7.13716670831516,-0.818376347595012,
1.53245209596733));
#11095=CARTESIAN_POINT('Ctrl Pts',(-6.82779061711728,-0.827560724830197,
1.54433902667896));
#11096=CARTESIAN_POINT('Ctrl Pts',(-6.47583393331273,-0.681911359548126,
1.55854925722825));
#11097=CARTESIAN_POINT('Ctrl Pts',(-6.21016594208147,-0.330954869083988,
1.57509380975784));
#11098=CARTESIAN_POINT('Ctrl Pts',(-6.14705675793353,0.0870687063999194,
1.59099390692264));
#11099=CARTESIAN_POINT('Ctrl Pts',(-6.29178381216594,0.484946937091849,
1.60691177329472));
#11100=CARTESIAN_POINT('Ctrl Pts',(-6.60953147959695,0.765383168267148,
1.62284694312522));
#11101=CARTESIAN_POINT('Ctrl Pts',(-7.02306130867876,0.859862600782519,
1.63879940878992));
#11102=CARTESIAN_POINT('Ctrl Pts',(-7.43209092835715,0.744843356641513,
1.65476878917197));
#11103=CARTESIAN_POINT('Ctrl Pts',(-7.7360822935237,0.448060979198733,1.67075513675566));
#11104=CARTESIAN_POINT('Ctrl Pts',(-7.87645764778973,-0.00385954133554831,
1.6885372052021));
#11105=CARTESIAN_POINT('Ctrl Pts',(-7.72834851689841,-0.516119382107579,
1.70812061510533));
#11106=CARTESIAN_POINT('Ctrl Pts',(-7.25468100412709,-0.856808986327443,
1.7295133131787));
#11107=CARTESIAN_POINT('Ctrl Pts',(-6.72053536605562,-0.834270555713778,
1.7491497241697));
#11108=CARTESIAN_POINT('Ctrl Pts',(-6.33474611188452,-0.555924840423259,
1.76701999702058));
#11109=CARTESIAN_POINT('Ctrl Pts',(-6.14885811639311,-0.170590221039593,
1.78311889654665));
#11110=CARTESIAN_POINT('Ctrl Pts',(-6.17018600999163,0.25761300576502,1.79923302183049));
#11111=CARTESIAN_POINT('Ctrl Pts',(-6.3938333344896,0.623621296817837,1.81536201710917));
#11112=CARTESIAN_POINT('Ctrl Pts',(-6.76559988585565,0.838322726739336,
1.83150595091894));
#11113=CARTESIAN_POINT('Ctrl Pts',(-7.19533204419046,0.849214134207467,
1.8476636842115));
#11114=CARTESIAN_POINT('Ctrl Pts',(-7.51408506059226,0.685479419534324,
1.86114130347342));
#11115=CARTESIAN_POINT('Ctrl Pts',(-7.69935073706812,0.475097794954268,
1.87193087421034));
#11116=CARTESIAN_POINT('Ctrl Pts',(-7.82756719690158,0.225696299951463,
1.88272501062167));
#11117=CARTESIAN_POINT('Ctrl Pts',(-7.86345218589821,-0.131510401233362,
1.8962239903695));
#11118=CARTESIAN_POINT('Ctrl Pts',(-7.69613807595462,-0.528918375423483,
1.91243912933416));
#11119=CARTESIAN_POINT('Ctrl Pts',(-7.35867518420911,-0.798157754455865,
1.9286640042301));
#11120=CARTESIAN_POINT('Ctrl Pts',(-6.96881533719357,-0.86658287393614,
1.94355059132535));
#11121=CARTESIAN_POINT('Ctrl Pts',(-6.62565014145497,-0.774407287161083,
1.95709390795204));
#11122=CARTESIAN_POINT('Ctrl Pts',(-6.36815349730449,-0.584571010932259,
1.96928914184098));
#11123=CARTESIAN_POINT('Ctrl Pts',(-6.19791761268333,-0.313459785840694,
1.9814915020885));
#11124=CARTESIAN_POINT('Ctrl Pts',(-6.13824564444744,0.00126222564801271,
1.99370039068808));
#11125=CARTESIAN_POINT('Ctrl Pts',(-6.19791470426975,0.316044722401465,
2.00591590248117));
#11126=CARTESIAN_POINT('Ctrl Pts',(-6.36840364468326,0.587805810914203,
2.01813791913327));
#11127=CARTESIAN_POINT('Ctrl Pts',(-6.62655450559938,0.777726269115704,
2.03036614812532));
#11128=CARTESIAN_POINT('Ctrl Pts',(-7.03995270037433,0.890005270964902,
2.04667918548612));
#11129=CARTESIAN_POINT('Ctrl Pts',(-7.57875104075548,0.724669890533431,
2.06708353353878));
#11130=CARTESIAN_POINT('Ctrl Pts',(-7.91803573835962,0.137269411407317,
2.09159331225351));
#11131=CARTESIAN_POINT('Ctrl Pts',(-7.76706117168378,-0.52400406240848,
2.1161247857463));
#11132=CARTESIAN_POINT('Ctrl Pts',(-7.20611421556751,-0.906687379904759,
2.14067751861688));
#11133=CARTESIAN_POINT('Ctrl Pts',(-6.53407310359242,-0.805456679357255,
2.16525004772343));
#11134=CARTESIAN_POINT('Ctrl Pts',(-6.10996474228539,-0.273794595356463,
2.18984134725865));
#11135=CARTESIAN_POINT('Ctrl Pts',(-6.16073373652603,0.404915665396,2.21445019333614));
#11136=CARTESIAN_POINT('Ctrl Pts',(-6.65992496701694,0.868206142671759,
2.23907543071713));
#11137=CARTESIAN_POINT('Ctrl Pts',(-7.34139465906004,0.868284001000674,
2.26371586031783));
#11138=CARTESIAN_POINT('Ctrl Pts',(-7.84127886499866,0.404554221629114,
2.28837028439299));
#11139=CARTESIAN_POINT('Ctrl Pts',(-7.89232330647337,-0.275743068898642,
2.31303748987548));
#11140=CARTESIAN_POINT('Ctrl Pts',(-7.46681769389894,-0.809401324879221,
2.33771625419332));
#11141=CARTESIAN_POINT('Ctrl Pts',(-6.79163727905948,-0.911218932362134,
2.36240534623989));
#11142=CARTESIAN_POINT('Ctrl Pts',(-6.22723819401461,-0.526470972456904,
2.38710352441179));
#11143=CARTESIAN_POINT('Ctrl Pts',(-6.07515776140191,0.139671239855932,
2.41180954160707));
#11144=CARTESIAN_POINT('Ctrl Pts',(-6.4168642269915,0.731580916682001,2.43652214117368));
#11145=CARTESIAN_POINT('Ctrl Pts',(-7.07009497004517,0.933103386959657,
2.46124006421744));
#11146=CARTESIAN_POINT('Ctrl Pts',(-7.6861192958364,0.63645551279314,2.48596203741659));
#11147=CARTESIAN_POINT('Ctrl Pts',(-7.93594161987389,-5.53991550515054E-5,
2.51068680546929));
#11148=CARTESIAN_POINT('Ctrl Pts',(-7.68613683601064,-0.636663310280273,
2.53541304689358));
#11149=CARTESIAN_POINT('Ctrl Pts',(-7.06997132216139,-0.933290058159735,
2.56013958420914));
#11150=CARTESIAN_POINT('Ctrl Pts',(-6.41666529744918,-0.731923724485437,
2.58486487069508));
#11151=CARTESIAN_POINT('Ctrl Pts',(-6.07456382672486,-0.139335588546712,
2.60958819020872));
#11152=CARTESIAN_POINT('Ctrl Pts',(-6.20189998741875,0.415187630242587,
2.63018704219427));
#11153=CARTESIAN_POINT('Ctrl Pts',(-6.50889656590471,0.720128182080066,
2.64666510151446));
#11154=CARTESIAN_POINT('Ctrl Pts',(-6.80552668601887,0.850092546186389,
2.65902201878275));
#11155=CARTESIAN_POINT('Ctrl Pts',(-7.12961665841912,0.862002494205028,
2.6713774719234));
#11156=CARTESIAN_POINT('Ctrl Pts',(-7.43548347744342,0.755101152634445,
2.68373125908594));
#11157=CARTESIAN_POINT('Ctrl Pts',(-7.68104236213469,0.543633793008857,
2.69608312748103));
#11158=CARTESIAN_POINT('Ctrl Pts',(-7.83254697985538,0.257228154096008,
2.70843323313999));
#11159=CARTESIAN_POINT('Ctrl Pts',(-7.86861092865602,-0.0646242885083314,
2.72078087920498));
#11160=CARTESIAN_POINT('Ctrl Pts',(-7.77114357730519,-0.429760638880875,
2.73518461873645));
#11161=CARTESIAN_POINT('Ctrl Pts',(-7.47768041418785,-0.759071075031029,
2.75164059738));
#11162=CARTESIAN_POINT('Ctrl Pts',(-7.00044547067498,-0.896286834016264,
2.77014692551625));
#11163=CARTESIAN_POINT('Ctrl Pts',(-6.52384755468618,-0.758970388215617,
2.78864723612747));
#11164=CARTESIAN_POINT('Ctrl Pts',(-6.19334012335843,-0.38912725030458,
2.80714040083053));
#11165=CARTESIAN_POINT('Ctrl Pts',(-6.1103571328977,0.0995956644790968,
2.82562612963652));
#11166=CARTESIAN_POINT('Ctrl Pts',(-6.30000871896293,0.557383043092008,
2.84410374158365));
#11167=CARTESIAN_POINT('Ctrl Pts',(-6.70395782539939,0.843960256355834,
2.86257284280838));
#11168=CARTESIAN_POINT('Ctrl Pts',(-7.1982573895186,0.871674220369247,2.88103270749344));
#11169=CARTESIAN_POINT('Ctrl Pts',(-7.63122519892655,0.632319691352436,
2.89948325375147));
#11170=CARTESIAN_POINT('Ctrl Pts',(-7.87057865226024,0.199460779002233,
2.91792304408701));
#11171=CARTESIAN_POINT('Ctrl Pts',(-7.84249835142399,-0.293910837809749,
2.93635365094154));
#11172=CARTESIAN_POINT('Ctrl Pts',(-7.55670690192362,-0.696723750004534,
2.95477217425725));
#11173=CARTESIAN_POINT('Ctrl Pts',(-7.10066709958465,-0.885581860171592,
2.97317926541403));
#11174=CARTESIAN_POINT('Ctrl Pts',(-6.61437502277845,-0.802910390411064,
2.99157433709339));
#11175=CARTESIAN_POINT('Ctrl Pts',(-6.24685080367674,-0.474398196000392,
3.00995694611218));
#11176=CARTESIAN_POINT('Ctrl Pts',(-6.11053734543688,-0.00103335347657871,
3.02832662126797));
#11177=CARTESIAN_POINT('Ctrl Pts',(-6.24686361423024,0.471957306655142,
3.04668290533691));
#11178=CARTESIAN_POINT('Ctrl Pts',(-6.61366423072175,0.799673263093506,
3.06502535163926));
#11179=CARTESIAN_POINT('Ctrl Pts',(-7.09821994184268,0.881944668383278,
3.08335351554756));
#11180=CARTESIAN_POINT('Ctrl Pts',(-7.55190977568874,0.693957832127035,
3.10166696504459));
#11181=CARTESIAN_POINT('Ctrl Pts',(-7.83580785554474,0.293739343295185,
3.11996527109821));
#11182=CARTESIAN_POINT('Ctrl Pts',(-7.86323708904419,-0.195759930573144,
3.13824801170802));
#11183=CARTESIAN_POINT('Ctrl Pts',(-7.62623911633122,-0.624446980074989,
3.15651477910607));
#11184=CARTESIAN_POINT('Ctrl Pts',(-7.19787659404976,-0.861121517451799,
3.17476516277629));
#11185=CARTESIAN_POINT('Ctrl Pts',(-6.70970363928432,-0.83364058160835,
3.19299876958912));
#11186=CARTESIAN_POINT('Ctrl Pts',(-6.31135370706244,-0.550913868799662,
3.21121520727279));
#11187=CARTESIAN_POINT('Ctrl Pts',(-6.12466269110821,-0.100022524381656,
3.22941409750615));
#11188=CARTESIAN_POINT('Ctrl Pts',(-6.20639624300564,0.380608586344866,
3.24759506582347));
#11189=CARTESIAN_POINT('Ctrl Pts',(-6.53098669794507,0.743718343207315,
3.26575774696197));
#11190=CARTESIAN_POINT('Ctrl Pts',(-6.99853026788513,0.878339630134887,
3.28390178877985));
#11191=CARTESIAN_POINT('Ctrl Pts',(-7.46554282551143,0.743718514945607,
3.30202684061782));
#11192=CARTESIAN_POINT('Ctrl Pts',(-7.78900382487124,0.381652261179626,
3.32013256737826));
#11193=CARTESIAN_POINT('Ctrl Pts',(-7.87016557654628,-0.0964892509804086,
3.33821863849062));
#11194=CARTESIAN_POINT('Ctrl Pts',(-7.68470472929137,-0.544027709032238,
3.35628473667664));
#11195=CARTESIAN_POINT('Ctrl Pts',(-7.29000983952638,-0.823982249810174,
3.3743305505273));
#11196=CARTESIAN_POINT('Ctrl Pts',(-6.80741892018219,-0.851004345886966,
3.39235577973309));
#11197=CARTESIAN_POINT('Ctrl Pts',(-6.38491355915793,-0.617402275389218,
3.41036013559038));
#11198=CARTESIAN_POINT('Ctrl Pts',(-6.15172476360541,-0.195316421174017,
3.42834333636049));
#11199=CARTESIAN_POINT('Ctrl Pts',(-6.17881634954805,0.285559220418923,
3.44630511117001));
#11200=CARTESIAN_POINT('Ctrl Pts',(-6.45724574362916,0.677841532703307,
3.4642452037166));
#11201=CARTESIAN_POINT('Ctrl Pts',(-6.90119282927497,0.861622534318975,
3.48216335628587));
#11202=CARTESIAN_POINT('Ctrl Pts',(-7.37421145008331,0.781158702191044,
3.50005935104225));
#11203=CARTESIAN_POINT('Ctrl Pts',(-7.73162808926433,0.461706158499515,
3.51793291265731));
#11204=CARTESIAN_POINT('Ctrl Pts',(-7.84174018381471,0.0784155713339669,
3.53280876811356));
#11205=CARTESIAN_POINT('Ctrl Pts',(-7.79800443241366,-0.227989827411191,
3.54469790503734));
#11206=CARTESIAN_POINT('Ctrl Pts',(-7.67204661082408,-0.51055230958309,
3.55657940142524));
#11207=CARTESIAN_POINT('Ctrl Pts',(-7.37563777804564,-0.775605435513216,
3.57141711961568));
#11208=CARTESIAN_POINT('Ctrl Pts',(-6.90521308169463,-0.855631913255045,
3.58919913713307));
#11209=CARTESIAN_POINT('Ctrl Pts',(-6.51465060638591,-0.69311751818218,
3.60498452681796));
#11210=CARTESIAN_POINT('Ctrl Pts',(-6.27881507231595,-0.418500796234524,
3.61878116804605));
#11211=CARTESIAN_POINT('Ctrl Pts',(-6.17632312766382,-0.126080287612221,
3.63059654719756));
#11212=CARTESIAN_POINT('Ctrl Pts',(-6.18805220951868,0.183382360639241,
3.64240124248303));
#11213=CARTESIAN_POINT('Ctrl Pts',(-6.31169162966109,0.466959088490852,
3.65419545058532));
#11214=CARTESIAN_POINT('Ctrl Pts',(-6.53036023200659,0.685431933329652,
3.66597892390944));
#11215=CARTESIAN_POINT('Ctrl Pts',(-6.81337429752307,0.808990321171382,
3.67775183119918));
#11216=CARTESIAN_POINT('Ctrl Pts',(-7.12172107959111,0.820464843886967,
3.68951368947386));
#11217=CARTESIAN_POINT('Ctrl Pts',(-7.34800121451071,0.741243120114073,
3.69865368566005));
#11218=CARTESIAN_POINT('Ctrl Pts',(-7.54454733227601,0.610797496612732,
3.70778790363217));
#11219=CARTESIAN_POINT('Ctrl Pts',(-7.72836238347323,0.407977213954234,
3.71822051453867));
#11220=CARTESIAN_POINT('Ctrl Pts',(-7.84066640889921,0.0439535641028487,
3.73255015514311));
#11221=CARTESIAN_POINT('Ctrl Pts',(-7.75492245715288,-0.38011715810829,
3.74881430963631));
#11222=CARTESIAN_POINT('Ctrl Pts',(-7.45331040205047,-0.717798573300966,
3.76570679042953));
#11223=CARTESIAN_POINT('Ctrl Pts',(-7.00184044230431,-0.847738465434875,
3.78322435324808));
#11224=CARTESIAN_POINT('Ctrl Pts',(-6.55122324812836,-0.717788116639949,
3.80071732111976));
#11225=CARTESIAN_POINT('Ctrl Pts',(-6.23916998145882,-0.368503730982292,
3.81818563971551));
#11226=CARTESIAN_POINT('Ctrl Pts',(-6.16095439337113,0.0926910769171822,
3.83562938690738));
#11227=CARTESIAN_POINT('Ctrl Pts',(-6.33974396233009,0.524030742822703,
3.8530484228516));
#11228=CARTESIAN_POINT('Ctrl Pts',(-6.72027090623596,0.794170891984653,
3.8704431308788));
#11229=CARTESIAN_POINT('Ctrl Pts',(-7.1334479191549,0.816691600475571,3.88588284353928));
#11230=CARTESIAN_POINT('Ctrl Pts',(-7.457766743847,0.67478730266217,3.89937585423884));
#11231=CARTESIAN_POINT('Ctrl Pts',(-7.67215648924734,0.46061316986074,3.91093083109438));
#11232=CARTESIAN_POINT('Ctrl Pts',(-7.79312888962497,0.182997472536088,
3.92247465031486));
#11233=CARTESIAN_POINT('Ctrl Pts',(-7.80451620006278,-0.119330813613606,
3.93400773053184));
#11234=CARTESIAN_POINT('Ctrl Pts',(-7.70459309568693,-0.404491448730027,
3.94552981955708));
#11235=CARTESIAN_POINT('Ctrl Pts',(-7.50767277094898,-0.633584373326835,
3.95704107739786));
#11236=CARTESIAN_POINT('Ctrl Pts',(-7.24100086035615,-0.773972195308569,
3.96854144986818));
#11237=CARTESIAN_POINT('Ctrl Pts',(-6.84150953053856,-0.820277435822203,
3.98386071903549));
#11238=CARTESIAN_POINT('Ctrl Pts',(-6.3654633640183,-0.591611081989893,
4.00298376177583));
#11239=CARTESIAN_POINT('Ctrl Pts',(-6.1337576390178,-0.00166122908455176,
4.02588709218193));
#11240=CARTESIAN_POINT('Ctrl Pts',(-6.36524032244932,0.586552139022073,
4.0487488089353));
#11241=CARTESIAN_POINT('Ctrl Pts',(-6.93373182771633,0.860206205841142,
4.07156736576551));
#11242=CARTESIAN_POINT('Ctrl Pts',(-7.53554145104219,0.674250442998106,
4.0943439987415));
#11243=CARTESIAN_POINT('Ctrl Pts',(-7.84970605920547,0.129907369813062,
4.11707862258703));
#11244=CARTESIAN_POINT('Ctrl Pts',(-7.70979429430066,-0.482242979932142,
4.13977201588358));
#11245=CARTESIAN_POINT('Ctrl Pts',(-7.24987944831994,-0.794866937844285,
4.1599071059334));
#11246=CARTESIAN_POINT('Ctrl Pts',(-6.78164215790337,-0.78159338937728,
4.17749998328314));
#11247=CARTESIAN_POINT('Ctrl Pts',(-6.43508142553994,-0.581914508121684,
4.19256186736058));
#11248=CARTESIAN_POINT('Ctrl Pts',(-6.22649440794211,-0.240291343540091,
4.20760570805015));
#11249=CARTESIAN_POINT('Ctrl Pts',(-6.20646282732663,0.158625568218903,
4.22263173846367));
#11250=CARTESIAN_POINT('Ctrl Pts',(-6.37985866256235,0.518181945746219,
4.23763986606553));
#11251=CARTESIAN_POINT('Ctrl Pts',(-6.676621959726,0.731271387526176,4.25138360802136));
#11252=CARTESIAN_POINT('Ctrl Pts',(-6.99833352149209,0.791913885519912,
4.26386326383385));
#11253=CARTESIAN_POINT('Ctrl Pts',(-7.28759771419049,0.737272473718823,
4.27508616182068));
#11254=CARTESIAN_POINT('Ctrl Pts',(-7.53651652643787,0.580727616932713,
4.2862994040904));
#11255=CARTESIAN_POINT('Ctrl Pts',(-7.71123812831514,0.344194682380573,
4.29750342874701));
#11256=CARTESIAN_POINT('Ctrl Pts',(-7.78672009233439,0.0608522761698529,
4.3086983822003));
#11257=CARTESIAN_POINT('Ctrl Pts',(-7.74407670626882,-0.328749819328367,
4.32361209918105));
#11258=CARTESIAN_POINT('Ctrl Pts',(-7.488016071979,-0.649656030398014,4.33851040798963));
#11259=CARTESIAN_POINT('Ctrl Pts',(-7.11855150721405,-0.77754314811613,
4.35338822144775));
#11260=CARTESIAN_POINT('Ctrl Pts',(-6.82669090383297,-0.767006673780784,
4.36453838462225));
#11261=CARTESIAN_POINT('Ctrl Pts',(-6.55873239018928,-0.649916384419054,
4.37567961202239));
#11262=CARTESIAN_POINT('Ctrl Pts',(-6.35226305448287,-0.443537303631106,
4.38681229399512));
#11263=CARTESIAN_POINT('Ctrl Pts',(-6.23566062987361,-0.176041345419126,
4.39793651633846));
#11264=CARTESIAN_POINT('Ctrl Pts',(-6.22467492822247,0.115336230842568,
4.40905210574612));
#11265=CARTESIAN_POINT('Ctrl Pts',(-6.32105446110734,0.390215990371737,
4.42015973648825));
#11266=CARTESIAN_POINT('Ctrl Pts',(-6.54241539602128,0.647903422644043,
4.4331081071576));
#11267=CARTESIAN_POINT('Ctrl Pts',(-6.90830837563262,0.800018879819483,
4.44789438520924));
#11268=CARTESIAN_POINT('Ctrl Pts',(-7.34773390300693,0.725076966311309,
4.46451191698296));
#11269=CARTESIAN_POINT('Ctrl Pts',(-7.67945563591345,0.428569859702225,
4.48111131802776));
#11270=CARTESIAN_POINT('Ctrl Pts',(-7.8025196238951,0.00128543290513052,
4.49769375395874));
#11271=CARTESIAN_POINT('Ctrl Pts',(-7.67949177727457,-0.425464330000851,
4.51425934408901));
#11272=CARTESIAN_POINT('Ctrl Pts',(-7.34861601444808,-0.721093459242237,
4.5308086687758));
#11273=CARTESIAN_POINT('Ctrl Pts',(-6.91158610847141,-0.795285145135524,
4.54734208939356));
#11274=CARTESIAN_POINT('Ctrl Pts',(-6.50245425438708,-0.625756719807303,
4.56386006942354));
#11275=CARTESIAN_POINT('Ctrl Pts',(-6.24645857835831,-0.26486761562661,
4.58036302642533));
#11276=CARTESIAN_POINT('Ctrl Pts',(-6.22172441041533,0.176514091733181,
4.59685141347568));
#11277=CARTESIAN_POINT('Ctrl Pts',(-6.43542969978214,0.563067075088938,
4.61332565034683));
#11278=CARTESIAN_POINT('Ctrl Pts',(-6.82170591717644,0.776505131784186,
4.62978623923995));
#11279=CARTESIAN_POINT('Ctrl Pts',(-7.26199738404331,0.75171591878271,4.64623352492646));
#11280=CARTESIAN_POINT('Ctrl Pts',(-7.62128776249611,0.496722562917399,
4.66266823384187));
#11281=CARTESIAN_POINT('Ctrl Pts',(-7.7898227412335,0.0898550976679472,
4.67909025716127));
#11282=CARTESIAN_POINT('Ctrl Pts',(-7.72819305262254,-0.271492440036806,
4.69276624996847));
#11283=CARTESIAN_POINT('Ctrl Pts',(-7.56970306360887,-0.5079089814104,4.70369975196043));
#11284=CARTESIAN_POINT('Ctrl Pts',(-7.35258106881955,-0.69180180336784,
4.71462953902306));
#11285=CARTESIAN_POINT('Ctrl Pts',(-7.00086436408432,-0.793298789487805,
4.7282869636663));
#11286=CARTESIAN_POINT('Ctrl Pts',(-6.5788579709131,-0.671628707119878,
4.74466442804047));
#11287=CARTESIAN_POINT('Ctrl Pts',(-6.28649729752278,-0.344430228222715,
4.76103233022189));
#11288=CARTESIAN_POINT('Ctrl Pts',(-6.21305030592735,0.0879749274087989,
4.77739058654941));
#11289=CARTESIAN_POINT('Ctrl Pts',(-6.38083417398137,0.492926507021418,
4.79373998172835));
#11290=CARTESIAN_POINT('Ctrl Pts',(-6.73816112992995,0.746427111490203,
4.81008089961082));
#11291=CARTESIAN_POINT('Ctrl Pts',(-7.17538345476371,0.770935644450725,
4.82641395115453));
#11292=CARTESIAN_POINT('Ctrl Pts',(-7.55845925877986,0.559185111777055,
4.84273956148575));
#11293=CARTESIAN_POINT('Ctrl Pts',(-7.77008458123184,0.176196391440457,
4.85905846124052));
#11294=CARTESIAN_POINT('Ctrl Pts',(-7.74552463470813,-0.260429333718453,
4.87537080311549));
#11295=CARTESIAN_POINT('Ctrl Pts',(-7.49255708704586,-0.617155518865413,
4.89167805198975));
#11296=CARTESIAN_POINT('Ctrl Pts',(-7.08868802008882,-0.784115034814167,
4.90797883579585));
#11297=CARTESIAN_POINT('Ctrl Pts',(-6.65800791988037,-0.711189244282659,
4.92427325384736));
#11298=CARTESIAN_POINT('Ctrl Pts',(-6.33230245467707,-0.419780727429073,
4.94056584505218));
#11299=CARTESIAN_POINT('Ctrl Pts',(-6.25175641581863,-0.140682475191443,
4.951421508845));
#11300=CARTESIAN_POINT('Ctrl Pts',(-6.2517375291819,-0.000258099276341313,
4.95685288349732));
#11301=CARTESIAN_POINT('Ctrl Pts',(-6.24478965756588,0.00137262626406237,
1.01435596443426));
#11302=CARTESIAN_POINT('Ctrl Pts',(-6.24480872457827,0.143138698890771,
1.01983923355613));
#11303=CARTESIAN_POINT('Ctrl Pts',(-6.32608128465411,0.424978386733189,
1.03079918563777));
#11304=CARTESIAN_POINT('Ctrl Pts',(-6.65521865496514,0.719545141515279,
1.047264334576));
#11305=CARTESIAN_POINT('Ctrl Pts',(-7.09084037841826,0.793351063930433,
1.06374450686311));
#11306=CARTESIAN_POINT('Ctrl Pts',(-7.49970099713228,0.624380947425885,
1.08024415418072));
#11307=CARTESIAN_POINT('Ctrl Pts',(-7.75600750517268,0.263001774579291,
1.096761015804));
#11308=CARTESIAN_POINT('Ctrl Pts',(-7.78094764461577,-0.179705724201667,
1.11329777783683));
#11309=CARTESIAN_POINT('Ctrl Pts',(-7.56624806034485,-0.568359320453272,
1.12985374800478));
#11310=CARTESIAN_POINT('Ctrl Pts',(-7.17722399158054,-0.783435275533458,
1.14642981113991));
#11311=CARTESIAN_POINT('Ctrl Pts',(-6.73292093230953,-0.75857359293873,
1.1630260405376));
#11312=CARTESIAN_POINT('Ctrl Pts',(-6.36935606333102,-0.500772560556008,
1.17964310078603));
#11313=CARTESIAN_POINT('Ctrl Pts',(-6.22723166621629,-0.157314762363655,
1.1935078779172));
#11314=CARTESIAN_POINT('Ctrl Pts',(-6.23575892336378,0.1316270733121,1.20461096131842));
#11315=CARTESIAN_POINT('Ctrl Pts',(-6.32317045688339,0.407351472690643,
1.21572123401303));
#11316=CARTESIAN_POINT('Ctrl Pts',(-6.57129460717402,0.685404517511721,
1.22962200624638));
#11317=CARTESIAN_POINT('Ctrl Pts',(-7.00177871327315,0.809460583789162,
1.24632536995202));
#11318=CARTESIAN_POINT('Ctrl Pts',(-7.43273340799708,0.68539316855628,1.26305104323195));
#11319=CARTESIAN_POINT('Ctrl Pts',(-7.73208724033317,0.350563465410518,
1.27979954233786));
#11320=CARTESIAN_POINT('Ctrl Pts',(-7.80749621963317,-0.0928033737312345,
1.29657108657474));
#11321=CARTESIAN_POINT('Ctrl Pts',(-7.63523348472294,-0.508921058338126,
1.31336601543416));
#11322=CARTESIAN_POINT('Ctrl Pts',(-7.26746462947776,-0.769973596782068,
1.33018460171811));
#11323=CARTESIAN_POINT('Ctrl Pts',(-6.81653894065146,-0.795387340746902,
1.34702713029165));
#11324=CARTESIAN_POINT('Ctrl Pts',(-6.42063877406979,-0.576685808156854,
1.36389386704994));
#11325=CARTESIAN_POINT('Ctrl Pts',(-6.20145878548216,-0.180301041143896,
1.38078506735707));
#11326=CARTESIAN_POINT('Ctrl Pts',(-6.22679890508924,0.272598213463161,
1.39770097937002));
#11327=CARTESIAN_POINT('Ctrl Pts',(-6.48959707258473,0.643145408485334,
1.41464183158308));
#11328=CARTESIAN_POINT('Ctrl Pts',(-6.90988024877083,0.817332105769404,
1.43160785087766));
#11329=CARTESIAN_POINT('Ctrl Pts',(-7.35908439929381,0.741116563166618,
1.44859923602708));
#11330=CARTESIAN_POINT('Ctrl Pts',(-7.69940105999772,0.437104669327555,
1.46561620559972));
#11331=CARTESIAN_POINT('Ctrl Pts',(-7.82599067828337,-0.00196328820679597,
1.48265889161566));
#11332=CARTESIAN_POINT('Ctrl Pts',(-7.69940416409236,-0.441905797127277,
1.4997275794512));
#11333=CARTESIAN_POINT('Ctrl Pts',(-7.41454913261973,-0.69629899338882,
1.51397305883405));
#11334=CARTESIAN_POINT('Ctrl Pts',(-7.13140667031658,-0.786088418557249,
1.52538288124777));
#11335=CARTESIAN_POINT('Ctrl Pts',(-6.83422969008724,-0.794912750226276,
1.53680147993686));
#11336=CARTESIAN_POINT('Ctrl Pts',(-6.49607200192091,-0.654985310754425,
1.55045570442471));
#11337=CARTESIAN_POINT('Ctrl Pts',(-6.2407524690546,-0.317718282519394,
1.56635617473815));
#11338=CARTESIAN_POINT('Ctrl Pts',(-6.18007554423253,0.0841108187200578,
1.58164154787721));
#11339=CARTESIAN_POINT('Ctrl Pts',(-6.31922227546523,0.466683776222355,
1.59694805597311));
#11340=CARTESIAN_POINT('Ctrl Pts',(-6.62482220448134,0.736416004700852,
1.61227569535595));
#11341=CARTESIAN_POINT('Ctrl Pts',(-7.02267006901935,0.827326148404722,
1.62762455399574));
#11342=CARTESIAN_POINT('Ctrl Pts',(-7.41631842058975,0.716646341891919,
1.64299464958104));
#11343=CARTESIAN_POINT('Ctrl Pts',(-7.70898346075156,0.430944328664958,
1.65838604777664));
#11344=CARTESIAN_POINT('Ctrl Pts',(-7.84418225096818,-0.00425490247512673,
1.67551144831122));
#11345=CARTESIAN_POINT('Ctrl Pts',(-7.70153133831721,-0.497784459731678,
1.69437976323737));
#11346=CARTESIAN_POINT('Ctrl Pts',(-7.24499583736429,-0.82620835645191,
1.71500140710803));
#11347=CARTESIAN_POINT('Ctrl Pts',(-6.72987671427024,-0.804517577019736,
1.73393944971573));
#11348=CARTESIAN_POINT('Ctrl Pts',(-6.35763389562258,-0.535974690110675,
1.75118344195896));
#11349=CARTESIAN_POINT('Ctrl Pts',(-6.17818960637836,-0.164043475609255,
1.76672440805754));
#11350=CARTESIAN_POINT('Ctrl Pts',(-6.19876227997895,0.249452063500465,
1.78228670600653));
#11351=CARTESIAN_POINT('Ctrl Pts',(-6.41480376192196,0.603053959900638,
1.79787030241971));
#11352=CARTESIAN_POINT('Ctrl Pts',(-6.77410654704341,0.810584525476164,
1.81347516452805));
#11353=CARTESIAN_POINT('Ctrl Pts',(-7.18964007933331,0.82113897670841,1.82910121659992));
#11354=CARTESIAN_POINT('Ctrl Pts',(-7.49801168006833,0.662761334008476,
1.84214058537142));
#11355=CARTESIAN_POINT('Ctrl Pts',(-7.67730194306007,0.459168604884869,
1.85258264275383));
#11356=CARTESIAN_POINT('Ctrl Pts',(-7.80141394481105,0.217757463993583,
1.86303171269498));
#11357=CARTESIAN_POINT('Ctrl Pts',(-7.83618078765266,-0.128153425658411,
1.87610615924427));
#11358=CARTESIAN_POINT('Ctrl Pts',(-7.67410372643082,-0.513175803930637,
1.89181646036404));
#11359=CARTESIAN_POINT('Ctrl Pts',(-7.34698936491175,-0.774192636346201,
1.90754760602515));
#11360=CARTESIAN_POINT('Ctrl Pts',(-6.96888724945337,-0.840575147748606,
1.92198684917859));
#11361=CARTESIAN_POINT('Ctrl Pts',(-6.63591501935329,-0.751154144255077,
1.93512845763984));
#11362=CARTESIAN_POINT('Ctrl Pts',(-6.38596089432625,-0.566886110545563,
1.94696750823183));
#11363=CARTESIAN_POINT('Ctrl Pts',(-6.2206329095347,-0.303620305915186,
1.95881805136626));
#11364=CARTESIAN_POINT('Ctrl Pts',(-6.16265528038784,0.00213076702521229,
1.97068009034218));
#11365=CARTESIAN_POINT('Ctrl Pts',(-6.22063155782939,0.308074592096969,
1.9825535218887));
#11366=CARTESIAN_POINT('Ctrl Pts',(-6.38639453550796,0.572318399981239,
1.99443833048481));
#11367=CARTESIAN_POINT('Ctrl Pts',(-6.63750082851633,0.757076300713128,
2.00633442846872));
#11368=CARTESIAN_POINT('Ctrl Pts',(-7.03979511845481,0.866354626682583,
2.02221086884604));
#11369=CARTESIAN_POINT('Ctrl Pts',(-7.56452076362568,0.705436392437274,
2.04208449694015));
#11370=CARTESIAN_POINT('Ctrl Pts',(-7.89532063815632,0.132955351120002,
2.06597694663177));
#11371=CARTESIAN_POINT('Ctrl Pts',(-7.74814558033186,-0.512206972690164,
2.08991303508929));
#11372=CARTESIAN_POINT('Ctrl Pts',(-7.20044035770089,-0.885999560658925,
2.11389211328061));
#11373=CARTESIAN_POINT('Ctrl Pts',(-6.54353829697939,-0.787170702788547,
2.13791356135016));
#11374=CARTESIAN_POINT('Ctrl Pts',(-6.12849619905038,-0.267069695319362,
2.1619766919057));
#11375=CARTESIAN_POINT('Ctrl Pts',(-6.17809374798513,0.39764412094938,2.1860807974792));
#11376=CARTESIAN_POINT('Ctrl Pts',(-6.6673876687898,0.851921518939688,2.21022512739177));
#11377=CARTESIAN_POINT('Ctrl Pts',(-7.3361417776358,0.85212632289709,2.23440890190676));
#11378=CARTESIAN_POINT('Ctrl Pts',(-7.82729157862744,0.396676944171653,
2.25863130495804));
#11379=CARTESIAN_POINT('Ctrl Pts',(-7.87761889481913,-0.272298298286383,
2.28289149000321));
#11380=CARTESIAN_POINT('Ctrl Pts',(-7.45885322696456,-0.797717856456593,
2.30718857710582));
#11381=CARTESIAN_POINT('Ctrl Pts',(-6.79351605019779,-0.898187779738267,
2.33152165675313));
#11382=CARTESIAN_POINT('Ctrl Pts',(-6.23665530172092,-0.518743940711026,
2.3558897879953));
#11383=CARTESIAN_POINT('Ctrl Pts',(-6.08633025914367,0.139089740107986,
2.38029200104115));
#11384=CARTESIAN_POINT('Ctrl Pts',(-6.42403744797426,0.724350123935663,
2.40472729859082));
#11385=CARTESIAN_POINT('Ctrl Pts',(-7.07051975136867,0.923937689560396,
2.42919465185401));
#11386=CARTESIAN_POINT('Ctrl Pts',(-7.68095292849436,0.630139560134256,
2.45369301454097));
#11387=CARTESIAN_POINT('Ctrl Pts',(-7.92888975457696,-0.00117722803999169,
2.4782212968774));
#11388=CARTESIAN_POINT('Ctrl Pts',(-7.68096129917293,-0.633397297572642,
2.50277842069243));
#11389=CARTESIAN_POINT('Ctrl Pts',(-7.06847078971012,-0.928413302755619,
2.52736321309282));
#11390=CARTESIAN_POINT('Ctrl Pts',(-6.41822884505462,-0.728138458316165,
2.55197463609316));
#11391=CARTESIAN_POINT('Ctrl Pts',(-6.07724055039059,-0.137772562194659,
2.57661128974893));
#11392=CARTESIAN_POINT('Ctrl Pts',(-6.2041537489263,0.415396542443843,2.59716234881447));
#11393=CARTESIAN_POINT('Ctrl Pts',(-6.5106186599655,0.719851428307833,2.61361411273135));
#11394=CARTESIAN_POINT('Ctrl Pts',(-6.8069155576107,0.849680046560568,2.62595864080187));
#11395=CARTESIAN_POINT('Ctrl Pts',(-7.13082962633578,0.861607082077237,
2.63830854948994));
#11396=CARTESIAN_POINT('Ctrl Pts',(-7.43670743335138,0.754714025872106,
2.650663745239));
#11397=CARTESIAN_POINT('Ctrl Pts',(-7.68242632568281,0.543140860474417,
2.6630240662951));
#11398=CARTESIAN_POINT('Ctrl Pts',(-7.83411705633228,0.256414360912654,
2.67538926259632));
#11399=CARTESIAN_POINT('Ctrl Pts',(-7.87026612947435,-0.0659867172657883,
2.68775937238401));
#11400=CARTESIAN_POINT('Ctrl Pts',(-7.77259819099482,-0.43194811180035,
2.70219621234534));
#11401=CARTESIAN_POINT('Ctrl Pts',(-7.47830389323134,-0.762275469718452,
2.71870351830232));
#11402=CARTESIAN_POINT('Ctrl Pts',(-6.99925195605143,-0.900083285520933,
2.73728406475897));
#11403=CARTESIAN_POINT('Ctrl Pts',(-6.52041326604491,-0.762186110272097,
2.75587330329622));
#11404=CARTESIAN_POINT('Ctrl Pts',(-6.18803904580033,-0.39035034183194,
2.77447098916387));
#11405=CARTESIAN_POINT('Ctrl Pts',(-6.10447020366487,0.10146170411541,2.79307644170198));
#11406=CARTESIAN_POINT('Ctrl Pts',(-6.29542840058373,0.562557359160062,
2.81168919265943));
#11407=CARTESIAN_POINT('Ctrl Pts',(-6.70258147662802,0.851479185427026,
2.83030860229007));
#11408=CARTESIAN_POINT('Ctrl Pts',(-7.20125170285735,0.879494684881194,
2.84893423819587));
#11409=CARTESIAN_POINT('Ctrl Pts',(-7.63843855328058,0.637876372913607,
2.86756526042035));
#11410=CARTESIAN_POINT('Ctrl Pts',(-7.88035809055516,0.200492755901659,
2.88620170890916));
#11411=CARTESIAN_POINT('Ctrl Pts',(-7.85202142204041,-0.29845876402528,
2.90484163379457));
#11412=CARTESIAN_POINT('Ctrl Pts',(-7.56280258302911,-0.706196902313995,
2.92348609265406));
#11413=CARTESIAN_POINT('Ctrl Pts',(-7.10087636837703,-0.897554955048048,
2.94213371595227));
#11414=CARTESIAN_POINT('Ctrl Pts',(-6.60788068228692,-0.813802367473543,
2.96078400814431));
#11415=CARTESIAN_POINT('Ctrl Pts',(-6.23496493305269,-0.480547788919674,
2.97943635760958));
#11416=CARTESIAN_POINT('Ctrl Pts',(-6.09650253414724,7.36349993946475E-5,
2.99809019969138));
#11417=CARTESIAN_POINT('Ctrl Pts',(-6.2349771181594,0.480720839648531,3.01674493477996));
#11418=CARTESIAN_POINT('Ctrl Pts',(-6.60795446695765,0.814029867378355,
3.0353999849881));
#11419=CARTESIAN_POINT('Ctrl Pts',(-7.10108735452254,0.897813287578576,
3.05405475688368));
#11420=CARTESIAN_POINT('Ctrl Pts',(-7.56318811110013,0.706400234832789,
3.07270866751176));
#11421=CARTESIAN_POINT('Ctrl Pts',(-7.85259769038108,0.298505122220334,
3.0913611271422));
#11422=CARTESIAN_POINT('Ctrl Pts',(-7.88062923610225,-0.200789655071514,
3.1100115462463));
#11423=CARTESIAN_POINT('Ctrl Pts',(-7.63875548568654,-0.638405253397185,
3.12865934584202));
#11424=CARTESIAN_POINT('Ctrl Pts',(-7.20120385804123,-0.880216540516199,
3.14730393314355));
#11425=CARTESIAN_POINT('Ctrl Pts',(-6.70216864962299,-0.852175853442006,
3.16594473064668));
#11426=CARTESIAN_POINT('Ctrl Pts',(-6.29463891881066,-0.562996383687711,
3.18458115237288));
#11427=CARTESIAN_POINT('Ctrl Pts',(-6.10347922938325,-0.101444039751134,
3.20321262271211));
#11428=CARTESIAN_POINT('Ctrl Pts',(-6.18715764055134,0.390920015575365,
3.2218385621182));
#11429=CARTESIAN_POINT('Ctrl Pts',(-6.51985614614286,0.763173480128891,
3.24045839411342));
#11430=CARTESIAN_POINT('Ctrl Pts',(-6.99943938334765,0.901311586483643,
3.25907155278571));
#11431=CARTESIAN_POINT('Ctrl Pts',(-7.4788207561827,0.763174459095097,3.27767746322422));
#11432=CARTESIAN_POINT('Ctrl Pts',(-7.81109001430734,0.391318815599289,
3.29627556485821));
#11433=CARTESIAN_POINT('Ctrl Pts',(-7.89455169682821,-0.100097497499467,
3.31486529320673));
#11434=CARTESIAN_POINT('Ctrl Pts',(-7.70386101556373,-0.560374101563154,
3.33344609458917));
#11435=CARTESIAN_POINT('Ctrl Pts',(-7.29772308555257,-0.848499476380384,
3.35201741342008));
#11436=CARTESIAN_POINT('Ctrl Pts',(-6.80081211472958,-0.876366978091514,
3.37057870182124));
#11437=CARTESIAN_POINT('Ctrl Pts',(-6.36548955539379,-0.635727002536597,
3.3891294188677));
#11438=CARTESIAN_POINT('Ctrl Pts',(-6.12506247397863,-0.200625629362112,
3.40766902775647));
#11439=CARTESIAN_POINT('Ctrl Pts',(-6.15296596486626,0.295384481659381,
3.4261969892632));
#11440=CARTESIAN_POINT('Ctrl Pts',(-6.44028359736047,0.700257943509883,
3.44471280120836));
#11441=CARTESIAN_POINT('Ctrl Pts',(-6.89868721845295,0.890065507075794,
3.46321589645446));
#11442=CARTESIAN_POINT('Ctrl Pts',(-7.38738863336506,0.806971596575828,
3.48170588292528));
#11443=CARTESIAN_POINT('Ctrl Pts',(-7.75686478742672,0.476791024583235,
3.50018199886897));
#11444=CARTESIAN_POINT('Ctrl Pts',(-7.87077084655038,0.0804024613658974,
3.51556731136463));
#11445=CARTESIAN_POINT('Ctrl Pts',(-7.82552947727927,-0.23659238310725,
3.52786749975938));
#11446=CARTESIAN_POINT('Ctrl Pts',(-7.69519368038569,-0.5289897821278,3.54016273392284));
#11447=CARTESIAN_POINT('Ctrl Pts',(-7.38837510797035,-0.803387247485029,
3.55552315287051));
#11448=CARTESIAN_POINT('Ctrl Pts',(-6.90118418722867,-0.886299313188514,
3.5739398176403));
#11449=CARTESIAN_POINT('Ctrl Pts',(-6.49650898219159,-0.717941960742899,
3.59029563609768));
#11450=CARTESIAN_POINT('Ctrl Pts',(-6.25206501413344,-0.43331791425204,
3.60459551222303));
#11451=CARTESIAN_POINT('Ctrl Pts',(-6.14579849826547,-0.13015196899678,
3.61684541182134));
#11452=CARTESIAN_POINT('Ctrl Pts',(-6.15795266437509,0.19077242396127,3.62908747996092));
#11453=CARTESIAN_POINT('Ctrl Pts',(-6.28619805958025,0.484932375558522,
3.64132188608379));
#11454=CARTESIAN_POINT('Ctrl Pts',(-6.51307671878171,0.711620993696904,
3.65354829509404));
#11455=CARTESIAN_POINT('Ctrl Pts',(-6.80679521079412,0.839861359046399,
3.66576675059935));
#11456=CARTESIAN_POINT('Ctrl Pts',(-7.12688353097587,0.851781090486876,
3.67797658128607));
#11457=CARTESIAN_POINT('Ctrl Pts',(-7.36183858408272,0.769528777517046,
3.68746696476958));
#11458=CARTESIAN_POINT('Ctrl Pts',(-7.56594880662315,0.634064450549118,
3.69695273716616));
#11459=CARTESIAN_POINT('Ctrl Pts',(-7.75687033874915,0.423412431286683,
3.70778844822587));
#11460=CARTESIAN_POINT('Ctrl Pts',(-7.87355733995844,0.0452323384499969,
3.72267558425976));
#11461=CARTESIAN_POINT('Ctrl Pts',(-7.78447031050978,-0.395461131106034,
3.73957714818353));
#11462=CARTESIAN_POINT('Ctrl Pts',(-7.47096649053771,-0.746487726578873,
3.75713652316082));
#11463=CARTESIAN_POINT('Ctrl Pts',(-7.00154760739981,-0.881615131689879,
3.77535066808487));
#11464=CARTESIAN_POINT('Ctrl Pts',(-6.53288168780712,-0.746479680578851,
3.79354393071519));
#11465=CARTESIAN_POINT('Ctrl Pts',(-6.20824074564234,-0.38313278099757,
3.81171592602832));
#11466=CARTESIAN_POINT('Ctrl Pts',(-6.12683791666095,0.0967518892725567,
3.82986637795763));
#11467=CARTESIAN_POINT('Ctrl Pts',(-6.31289814013408,0.54567365371964,3.84799484839867));
#11468=CARTESIAN_POINT('Ctrl Pts',(-6.70899549333688,0.826886830764423,
3.86610127239849));
#11469=CARTESIAN_POINT('Ctrl Pts',(-7.1391642414818,0.850345684068663,3.88217553454808));
#11470=CARTESIAN_POINT('Ctrl Pts',(-7.4768673421196,0.702589166960476,3.89622519848683));
#11471=CARTESIAN_POINT('Ctrl Pts',(-7.70012720867177,0.479560881685281,
3.90825775646689));
#11472=CARTESIAN_POINT('Ctrl Pts',(-7.82611602300347,0.190439595430187,
3.92027984885091));
#11473=CARTESIAN_POINT('Ctrl Pts',(-7.83798099860797,-0.124443748955779,
3.93229155432904));
#11474=CARTESIAN_POINT('Ctrl Pts',(-7.73390245891118,-0.42146765183984,
3.94429271213602));
#11475=CARTESIAN_POINT('Ctrl Pts',(-7.52878052100635,-0.660108593551094,
3.95628324000648));
#11476=CARTESIAN_POINT('Ctrl Pts',(-7.25098324922026,-0.806353878555257,
3.96826309127496));
#11477=CARTESIAN_POINT('Ctrl Pts',(-6.83480606708229,-0.854597995909426,
3.98422176505027));
#11478=CARTESIAN_POINT('Ctrl Pts',(-6.33885148673084,-0.616373789874939,
4.00414345770479));
#11479=CARTESIAN_POINT('Ctrl Pts',(-6.09743829689286,-0.00172692772890619,
4.02800487858787));
#11480=CARTESIAN_POINT('Ctrl Pts',(-6.33861415409186,0.611112211811564,
4.05182224683903));
#11481=CARTESIAN_POINT('Ctrl Pts',(-6.930890647855,0.896211711923622,4.07559426239331));
#11482=CARTESIAN_POINT('Ctrl Pts',(-7.5578355247161,0.702480238617824,4.09932083585418));
#11483=CARTESIAN_POINT('Ctrl Pts',(-7.88507859972884,0.135449505681517,
4.12300136072554));
#11484=CARTESIAN_POINT('Ctrl Pts',(-7.73933983592004,-0.502118403477305,
4.14663556803947));
#11485=CARTESIAN_POINT('Ctrl Pts',(-7.26039367113424,-0.827655820518871,
4.16760211727223));
#11486=CARTESIAN_POINT('Ctrl Pts',(-6.77288173277215,-0.813828340996825,
4.18591758737132));
#11487=CARTESIAN_POINT('Ctrl Pts',(-6.41210932711652,-0.605956030043776,
4.20159558574628));
#11488=CARTESIAN_POINT('Ctrl Pts',(-6.19501402257771,-0.250376696431912,
4.21725247157529));
#11489=CARTESIAN_POINT('Ctrl Pts',(-6.17417056259732,0.164760155164131,
4.23288813280655));
#11490=CARTESIAN_POINT('Ctrl Pts',(-6.3545942969234,0.538855542040888,4.24850255309216));
#11491=CARTESIAN_POINT('Ctrl Pts',(-6.66328617817794,0.760507888724256,
4.26279661491745));
#11492=CARTESIAN_POINT('Ctrl Pts',(-6.9978784626736,0.823569792509618,4.27577535769565));
#11493=CARTESIAN_POINT('Ctrl Pts',(-7.29866400314611,0.766751391781709,
4.28744432659339));
#11494=CARTESIAN_POINT('Ctrl Pts',(-7.55744540147431,0.603995266851033,
4.29910128219956));
#11495=CARTESIAN_POINT('Ctrl Pts',(-7.73905541731227,0.358135252089175,
4.31074622431009));
#11496=CARTESIAN_POINT('Ctrl Pts',(-7.81749152608428,0.0636809190910327,
4.3223791871992));
#11497=CARTESIAN_POINT('Ctrl Pts',(-7.77317917381171,-0.341116140474648,
4.33787368203927));
#11498=CARTESIAN_POINT('Ctrl Pts',(-7.50721032388302,-0.674391183617128,
4.35334442702289));
#11499=CARTESIAN_POINT('Ctrl Pts',(-7.12360277329797,-0.807159429383535,
4.36879085079072));
#11500=CARTESIAN_POINT('Ctrl Pts',(-6.82064966915069,-0.79622001697244,
4.38036369654546));
#11501=CARTESIAN_POINT('Ctrl Pts',(-6.54258356263728,-0.674699950250188,
4.39192452633223));
#11502=CARTESIAN_POINT('Ctrl Pts',(-6.32838183258931,-0.460587210838161,
4.40347334046582));
#11503=CARTESIAN_POINT('Ctrl Pts',(-6.20745638360056,-0.183141123111028,
4.4150101887781));
#11504=CARTESIAN_POINT('Ctrl Pts',(-6.19607090850112,0.118985454375757,
4.42653502983482));
#11505=CARTESIAN_POINT('Ctrl Pts',(-6.29598849817137,0.40391719529154,4.43804794900205));
#11506=CARTESIAN_POINT('Ctrl Pts',(-6.52539085352358,0.670952624756736,
4.45146570163604));
#11507=CARTESIAN_POINT('Ctrl Pts',(-6.90442160364007,0.828498869433625,
4.46678049304922));
#11508=CARTESIAN_POINT('Ctrl Pts',(-7.35937715782801,0.75087237148055,4.48398292034035));
#11509=CARTESIAN_POINT('Ctrl Pts',(-7.70263994562715,0.444003510586905,
4.50115870290066));
#11510=CARTESIAN_POINT('Ctrl Pts',(-7.82989303341533,0.00204106946231624,
4.51830796948457));
#11511=CARTESIAN_POINT('Ctrl Pts',(-7.70267552148953,-0.43911345287367,
4.53543083756206));
#11512=CARTESIAN_POINT('Ctrl Pts',(-7.36078794810659,-0.74453315607766,
4.55252744875789));
#11513=CARTESIAN_POINT('Ctrl Pts',(-6.90949624334495,-0.821109089414126,
4.56959794960374));
#11514=CARTESIAN_POINT('Ctrl Pts',(-6.48728069604972,-0.646119024648585,
4.58664250216479));
#11515=CARTESIAN_POINT('Ctrl Pts',(-6.22328014245951,-0.273879047789936,
4.60366128068545));
#11516=CARTESIAN_POINT('Ctrl Pts',(-6.19782444473162,0.181078373118608,
4.62065446856178));
#11517=CARTESIAN_POINT('Ctrl Pts',(-6.41799641702055,0.5792458930126,4.63762226650895));
#11518=CARTESIAN_POINT('Ctrl Pts',(-6.81565826960756,0.798929031456019,
4.6545648765693));
#11519=CARTESIAN_POINT('Ctrl Pts',(-7.26859902401305,0.773385786288969,
4.67148253456703));
#11520=CARTESIAN_POINT('Ctrl Pts',(-7.63793616170917,0.511211936303308,
4.68837544184199));
#11521=CARTESIAN_POINT('Ctrl Pts',(-7.81103129278376,0.0932135444940163,
4.7052439075552));
#11522=CARTESIAN_POINT('Ctrl Pts',(-7.74772659633056,-0.277723366438459,
4.71928068135095));
#11523=CARTESIAN_POINT('Ctrl Pts',(-7.58510165644112,-0.520294036256702,
4.73049830024372));
#11524=CARTESIAN_POINT('Ctrl Pts',(-7.36239850996586,-0.708904500801799,
4.74170798257738));
#11525=CARTESIAN_POINT('Ctrl Pts',(-7.00186095481488,-0.812908884827261,
4.75570503351309));
#11526=CARTESIAN_POINT('Ctrl Pts',(-6.56961433191529,-0.688237747232737,
4.77247823631829));
#11527=CARTESIAN_POINT('Ctrl Pts',(-6.27042017705918,-0.353314214709758,
4.78922830449849));
#11528=CARTESIAN_POINT('Ctrl Pts',(-6.19535597538779,0.0889191605106485,
4.80595562242244));
#11529=CARTESIAN_POINT('Ctrl Pts',(-6.36686335581866,0.502719028652008,
4.8226604694237));
#11530=CARTESIAN_POINT('Ctrl Pts',(-6.73175256486973,0.761520072268675,
4.83934320448615));
#11531=CARTESIAN_POINT('Ctrl Pts',(-7.17782997977493,0.786473326771477,
4.85600412593016));
#11532=CARTESIAN_POINT('Ctrl Pts',(-7.5683126081094,0.57057171907611,4.87264365440957));
#11533=CARTESIAN_POINT('Ctrl Pts',(-7.78382263552961,0.180461387737065,
4.88926197808321));
#11534=CARTESIAN_POINT('Ctrl Pts',(-7.75878282229075,-0.263872752181399,
4.90585981848288));
#11535=CARTESIAN_POINT('Ctrl Pts',(-7.50154978164387,-0.626551986690765,
4.92243671953082));
#11536=CARTESIAN_POINT('Ctrl Pts',(-7.09124424921979,-0.796114951309141,
4.93899483030102));
#11537=CARTESIAN_POINT('Ctrl Pts',(-6.65411810003208,-0.722048191241108,
4.95553216226915));
#11538=CARTESIAN_POINT('Ctrl Pts',(-6.32387059158365,-0.426484570176635,
4.97205308357914));
#11539=CARTESIAN_POINT('Ctrl Pts',(-6.24232917383988,-0.143709849746694,
4.98304959780136));
#11540=CARTESIAN_POINT('Ctrl Pts',(-6.24231004509627,-0.00148538057916514,
4.98855059698146));
#11541=CARTESIAN_POINT('Ctrl Pts',(-6.25574144158882,-0.000498857481043991,
1.06270377973105));
#11542=CARTESIAN_POINT('Ctrl Pts',(-6.25576022828242,0.139183003238407,
1.06810643510251));
#11543=CARTESIAN_POINT('Ctrl Pts',(-6.33586682667619,0.416721998384859,
1.07890094002148));
#11544=CARTESIAN_POINT('Ctrl Pts',(-6.65959485848297,0.706318708188977,
1.09509298618406));
#11545=CARTESIAN_POINT('Ctrl Pts',(-7.08739810828336,0.778721847560845,
1.11127784875485));
#11546=CARTESIAN_POINT('Ctrl Pts',(-7.48832794984565,0.612939978136046,
1.1274597570632));
#11547=CARTESIAN_POINT('Ctrl Pts',(-7.73928794456948,0.258977919487233,
1.14363817134105));
#11548=CARTESIAN_POINT('Ctrl Pts',(-7.76360338401286,-0.174005578196651,
1.15981328783718));
#11549=CARTESIAN_POINT('Ctrl Pts',(-7.55383634477513,-0.553573253430915,
1.17598591488793));
#11550=CARTESIAN_POINT('Ctrl Pts',(-7.17433261104523,-0.76329584980855,
1.19215651921613));
#11551=CARTESIAN_POINT('Ctrl Pts',(-6.74151458194365,-0.738996757692014,
1.20832585703833));
#11552=CARTESIAN_POINT('Ctrl Pts',(-6.38784581103617,-0.488116990817084,
1.22449424575166));
#11553=CARTESIAN_POINT('Ctrl Pts',(-6.24980489864987,-0.15436255814959,
1.23796812666697));
#11554=CARTESIAN_POINT('Ctrl Pts',(-6.25809489187119,0.126118231152519,
1.24874671827879));
#11555=CARTESIAN_POINT('Ctrl Pts',(-6.34290773639547,0.393603166796141,
1.25952554349459));
#11556=CARTESIAN_POINT('Ctrl Pts',(-6.58345162450279,0.663066705711368,
1.27300057006987));
#11557=CARTESIAN_POINT('Ctrl Pts',(-7.00020483358905,0.783086765045414,
1.28917173167979));
#11558=CARTESIAN_POINT('Ctrl Pts',(-7.41687065522309,0.663059338011621,
1.30534521235595));
#11559=CARTESIAN_POINT('Ctrl Pts',(-7.70591544232305,0.339653901481795,
1.3215213522553));
#11560=CARTESIAN_POINT('Ctrl Pts',(-7.77858712938061,-0.0880332025193281,
1.33770084993892));
#11561=CARTESIAN_POINT('Ctrl Pts',(-7.61254839496213,-0.488936729999324,
1.35388424102803));
#11562=CARTESIAN_POINT('Ctrl Pts',(-7.25856334262776,-0.740122115944731,
1.37007213360199));
#11563=CARTESIAN_POINT('Ctrl Pts',(-6.82506267309524,-0.764487181544599,
1.38626509399126));
#11564=CARTESIAN_POINT('Ctrl Pts',(-6.44490903164376,-0.554409724240902,
1.40246370734102));
#11565=CARTESIAN_POINT('Ctrl Pts',(-6.23470889983783,-0.174132948159932,
1.41866854181864));
#11566=CARTESIAN_POINT('Ctrl Pts',(-6.25905438180472,0.259870837709405,
1.43488017508944));
#11567=CARTESIAN_POINT('Ctrl Pts',(-6.51068392324855,0.614564502512315,
1.45109917288617));
#11568=CARTESIAN_POINT('Ctrl Pts',(-6.91264883964463,0.78109446323033,1.46732609435233));
#11569=CARTESIAN_POINT('Ctrl Pts',(-7.34182339671781,0.708217790535654,
1.48356152351232));
#11570=CARTESIAN_POINT('Ctrl Pts',(-7.66662800022932,0.417986725042806,
1.49980597216501));
#11571=CARTESIAN_POINT('Ctrl Pts',(-7.7872969698189,-0.000747736846312889,
1.51606009973265));
#11572=CARTESIAN_POINT('Ctrl Pts',(-7.6666342868507,-0.419909780883938,
1.53232423514785));
#11573=CARTESIAN_POINT('Ctrl Pts',(-7.39543041252767,-0.662055716649145,
1.54588691377005));
#11574=CARTESIAN_POINT('Ctrl Pts',(-7.12606123934068,-0.747468998803105,
1.55674207242413));
#11575=CARTESIAN_POINT('Ctrl Pts',(-6.84345620821393,-0.755852189904183,
1.56760104700489));
#11576=CARTESIAN_POINT('Ctrl Pts',(-6.5220837749257,-0.622828513848678,
1.58057931637516));
#11577=CARTESIAN_POINT('Ctrl Pts',(-6.27964104193747,-0.302511596729687,
1.59568049942823));
#11578=CARTESIAN_POINT('Ctrl Pts',(-6.2220864354709,0.0788440259113018,
1.61018790303456));
#11579=CARTESIAN_POINT('Ctrl Pts',(-6.35408418226561,0.441670066477265,
1.62470565559779));
#11580=CARTESIAN_POINT('Ctrl Pts',(-6.64375339876684,0.697301801776668,
1.63923425150086));
#11581=CARTESIAN_POINT('Ctrl Pts',(-7.0206119357728,0.783386360219316,1.65377397435476));
#11582=CARTESIAN_POINT('Ctrl Pts',(-7.39325720437512,0.678581967567608,
1.6683252500628));
#11583=CARTESIAN_POINT('Ctrl Pts',(-7.67013870264448,0.408254260386592,
1.68288834541239));
#11584=CARTESIAN_POINT('Ctrl Pts',(-7.79795365163416,-0.0032820587900806,
1.6990827439662));
#11585=CARTESIAN_POINT('Ctrl Pts',(-7.66309442919013,-0.469667500024928,
1.71691460045667));
#11586=CARTESIAN_POINT('Ctrl Pts',(-7.23190668680682,-0.779785048350367,
1.73639051607248));
#11587=CARTESIAN_POINT('Ctrl Pts',(-6.74573184654296,-0.759267380311345,
1.75426513540613));
#11588=CARTESIAN_POINT('Ctrl Pts',(-6.39459107302207,-0.505920169111814,
1.77053310370253));
#11589=CARTESIAN_POINT('Ctrl Pts',(-6.2253973160446,-0.155195481687715,
1.7851883329396));
#11590=CARTESIAN_POINT('Ctrl Pts',(-6.24480623004818,0.234563730110018,
1.79985798765964));
#11591=CARTESIAN_POINT('Ctrl Pts',(-6.44838629115469,0.567738725777836,
1.81454239612435));
#11592=CARTESIAN_POINT('Ctrl Pts',(-6.78683423413161,0.763206916772546,
1.82924177771278));
#11593=CARTESIAN_POINT('Ctrl Pts',(-7.17811932257024,0.773131221068672,
1.84395664824561));
#11594=CARTESIAN_POINT('Ctrl Pts',(-7.46840416020655,0.6240316513085,1.8562317924873));
#11595=CARTESIAN_POINT('Ctrl Pts',(-7.63714510399363,0.432414888572534,
1.86605972191242));
#11596=CARTESIAN_POINT('Ctrl Pts',(-7.75393931700189,0.205233365517019,
1.8758930057902));
#11597=CARTESIAN_POINT('Ctrl Pts',(-7.78664215748584,-0.120233197607642,
1.88819523160421));
#11598=CARTESIAN_POINT('Ctrl Pts',(-7.63417045939035,-0.482409153902618,
1.90297364848866));
#11599=CARTESIAN_POINT('Ctrl Pts',(-7.32651359382278,-0.72789070482646,
1.91776950585886));
#11600=CARTESIAN_POINT('Ctrl Pts',(-6.97097117673883,-0.790305576233221,
1.93134746236838));
#11601=CARTESIAN_POINT('Ctrl Pts',(-6.65790957425775,-0.706229485674086,
1.94370343248341));
#11602=CARTESIAN_POINT('Ctrl Pts',(-6.42292495799198,-0.532993864392855,
1.95483369581103));
#11603=CARTESIAN_POINT('Ctrl Pts',(-6.26751159004392,-0.285514108223224,
1.96597379393668));
#11604=CARTESIAN_POINT('Ctrl Pts',(-6.21301625364804,0.00188292046488118,
1.97712387179597));
#11605=CARTESIAN_POINT('Ctrl Pts',(-6.2675090658162,0.289443762118776,1.98828402919144));
#11606=CARTESIAN_POINT('Ctrl Pts',(-6.42330583078288,0.537798456401413,
1.99945431517307));
#11607=CARTESIAN_POINT('Ctrl Pts',(-6.65930551885432,0.7114420938548,2.01063488878302));
#11608=CARTESIAN_POINT('Ctrl Pts',(-7.03739094524968,0.814143836989083,
2.02555601312736));
#11609=CARTESIAN_POINT('Ctrl Pts',(-7.53053768011085,0.662913683709486,
2.04423381193589));
#11610=CARTESIAN_POINT('Ctrl Pts',(-7.84144903768382,0.124870379518979,
2.06668933863783));
#11611=CARTESIAN_POINT('Ctrl Pts',(-7.70312872983905,-0.481547002699999,
2.0891879441913));
#11612=CARTESIAN_POINT('Ctrl Pts',(-7.1882562937634,-0.832958294320995,
2.11173012604567));
#11613=CARTESIAN_POINT('Ctrl Pts',(-6.57059338007734,-0.740060748597092,
2.13431650032462));
#11614=CARTESIAN_POINT('Ctrl Pts',(-6.1802232556478,-0.250930801799442,
2.15694757743791));
#11615=CARTESIAN_POINT('Ctrl Pts',(-6.22684370912928,0.374415923588821,
2.17962385701603));
#11616=CARTESIAN_POINT('Ctrl Pts',(-6.68728605866362,0.801968733566327,
2.20234578920383));
#11617=CARTESIAN_POINT('Ctrl Pts',(-7.31689820140758,0.802213040629406,
2.22511378940577));
#11618=CARTESIAN_POINT('Ctrl Pts',(-7.77954577036186,0.373272342681926,
2.24792823286914));
#11619=CARTESIAN_POINT('Ctrl Pts',(-7.82703482894681,-0.257133770025224,
2.27078945587098));
#11620=CARTESIAN_POINT('Ctrl Pts',(-7.43225046320483,-0.752574828411877,
2.29369775546632));
#11621=CARTESIAN_POINT('Ctrl Pts',(-6.80457236171091,-0.847433409521687,
2.31665338874161));
#11622=CARTESIAN_POINT('Ctrl Pts',(-6.27884387479177,-0.489300063191618,
2.33965657329448));
#11623=CARTESIAN_POINT('Ctrl Pts',(-6.13675540828559,0.132104889847011,
2.36270748645569));
#11624=CARTESIAN_POINT('Ctrl Pts',(-6.45592275124396,0.685417394331864,
2.38580626524834));
#11625=CARTESIAN_POINT('Ctrl Pts',(-7.06750462557763,0.874331252516317,
2.40895300717511));
#11626=CARTESIAN_POINT('Ctrl Pts',(-7.64552182519084,0.596247683724882,
2.43214776683914));
#11627=CARTESIAN_POINT('Ctrl Pts',(-7.88057376599971,-0.00196814628072304,
2.45539056393457));
#11628=CARTESIAN_POINT('Ctrl Pts',(-7.64552409477716,-0.601654948176037,
2.47868136373957));
#11629=CARTESIAN_POINT('Ctrl Pts',(-7.06410018348824,-0.881837376955094,
2.50202012163737));
#11630=CARTESIAN_POINT('Ctrl Pts',(-6.44615034947898,-0.691637521520468,
2.52540667870236));
#11631=CARTESIAN_POINT('Ctrl Pts',(-6.12167515050772,-0.130120742172608,
2.54884100103956));
#11632=CARTESIAN_POINT('Ctrl Pts',(-6.24242004156193,0.396652017996355,
2.56840901450238));
#11633=CARTESIAN_POINT('Ctrl Pts',(-6.53447535363075,0.686823681480564,
2.58408734767232));
#11634=CARTESIAN_POINT('Ctrl Pts',(-6.81699805059676,0.810635681023223,
2.59585781985285));
#11635=CARTESIAN_POINT('Ctrl Pts',(-7.12603611624708,0.822030492458687,
2.60764008421422));
#11636=CARTESIAN_POINT('Ctrl Pts',(-7.41803788514657,0.72000683301485,2.61943404873999));
#11637=CARTESIAN_POINT('Ctrl Pts',(-7.65274995755222,0.517929884868489,
2.63123970145475));
#11638=CARTESIAN_POINT('Ctrl Pts',(-7.79774172107598,0.243906477114829,
2.64305702599696));
#11639=CARTESIAN_POINT('Ctrl Pts',(-7.83232527997599,-0.0644032051053991,
2.65488589026192));
#11640=CARTESIAN_POINT('Ctrl Pts',(-7.73889023355586,-0.414589190311789,
2.66869990431192));
#11641=CARTESIAN_POINT('Ctrl Pts',(-7.45711558261939,-0.730943004383703,
2.68450617152468));
#11642=CARTESIAN_POINT('Ctrl Pts',(-6.99796978668839,-0.863090579444672,
2.70231373581129));
#11643=CARTESIAN_POINT('Ctrl Pts',(-6.53855217084151,-0.730852022510803,
2.72014697009195));
#11644=CARTESIAN_POINT('Ctrl Pts',(-6.21931412255978,-0.373809109467704,
2.73800549127301));
#11645=CARTESIAN_POINT('Ctrl Pts',(-6.13891465776656,0.0989486782214521,
2.7558891571914));
#11646=CARTESIAN_POINT('Ctrl Pts',(-6.32259891652746,0.542660491028362,
2.77379768621757));
#11647=CARTESIAN_POINT('Ctrl Pts',(-6.71473487923161,0.821012435181475,
2.79173089130173));
#11648=CARTESIAN_POINT('Ctrl Pts',(-7.19555373615558,0.848098151534184,
2.80968842316349));
#11649=CARTESIAN_POINT('Ctrl Pts',(-7.61756823154174,0.614945844011524,
2.82767022347362));
#11650=CARTESIAN_POINT('Ctrl Pts',(-7.85138514701445,0.192369550326599,
2.84567556880744));
#11651=CARTESIAN_POINT('Ctrl Pts',(-7.82404608394165,-0.290269192588259,
2.86370517231971));
#11652=CARTESIAN_POINT('Ctrl Pts',(-7.54405162406482,-0.685136423624603,
2.88175754722335));
#11653=CARTESIAN_POINT('Ctrl Pts',(-7.09629257868619,-0.870707936190149,
2.89983297266089));
#11654=CARTESIAN_POINT('Ctrl Pts',(-6.61784180407662,-0.789503998643947,
2.91793106339489));
#11655=CARTESIAN_POINT('Ctrl Pts',(-6.25547880694769,-0.465783876765169,
2.9360515100578));
#11656=CARTESIAN_POINT('Ctrl Pts',(-6.12072563265172,0.00167905711825161,
2.95419397011278));
#11657=CARTESIAN_POINT('Ctrl Pts',(-6.25549336745657,0.46974689465823,2.97235809483517));
#11658=CARTESIAN_POINT('Ctrl Pts',(-6.61905883922182,0.794752880995018,
2.9905435289329));
#11659=CARTESIAN_POINT('Ctrl Pts',(-7.10036600226087,0.876609499720008,
3.0087499032196));
#11660=CARTESIAN_POINT('Ctrl Pts',(-7.55195993204527,0.689637344969144,
3.0269768429918));
#11661=CARTESIAN_POINT('Ctrl Pts',(-7.83517221510059,0.29061953446048,3.04522396103687));
#11662=CARTESIAN_POINT('Ctrl Pts',(-7.86271284952522,-0.198445949703901,
3.06349085934156));
#11663=CARTESIAN_POINT('Ctrl Pts',(-7.6255807553781,-0.627655924321167,
3.08177713801619));
#11664=CARTESIAN_POINT('Ctrl Pts',(-7.19599570183822,-0.865160948375789,
3.100082377186));
#11665=CARTESIAN_POINT('Ctrl Pts',(-6.70539880249602,-0.837679482344607,
3.11840615795295));
#11666=CARTESIAN_POINT('Ctrl Pts',(-6.30422426083902,-0.553114363892535,
3.13674804536529));
#11667=CARTESIAN_POINT('Ctrl Pts',(-6.11575799788189,-0.0982897902643771,
3.15510760179694));
#11668=CARTESIAN_POINT('Ctrl Pts',(-6.19823939872231,0.387546459541662,
3.17348437694896));
#11669=CARTESIAN_POINT('Ctrl Pts',(-6.52685982154688,0.755367181396514,
3.19187791210836));
#11670=CARTESIAN_POINT('Ctrl Pts',(-7.00122376758996,0.892092600222727,
3.21028774728281));
#11671=CARTESIAN_POINT('Ctrl Pts',(-7.47602897177808,0.755365132384686,
3.22871340448373));
#11672=CARTESIAN_POINT('Ctrl Pts',(-7.80558752389931,0.386674816692687,
3.24715440718115));
#11673=CARTESIAN_POINT('Ctrl Pts',(-7.8885426204605,-0.101233380981048,
3.26561026530892));
#11674=CARTESIAN_POINT('Ctrl Pts',(-7.69905050675687,-0.558847314582516,
3.28408048670801));
#11675=CARTESIAN_POINT('Ctrl Pts',(-7.29483346934859,-0.845718266442943,
3.3025645681768));
#11676=CARTESIAN_POINT('Ctrl Pts',(-6.79959008958347,-0.873580860447485,
3.32106199909265));
#11677=CARTESIAN_POINT('Ctrl Pts',(-6.36513240365607,-0.633520245208162,
3.33957227042389));
#11678=CARTESIAN_POINT('Ctrl Pts',(-6.12482522958441,-0.198819481209487,
3.35809485071837));
#11679=CARTESIAN_POINT('Ctrl Pts',(-6.15265228854888,0.297415232772545,
3.37662922508223));
#11680=CARTESIAN_POINT('Ctrl Pts',(-6.44038811710877,0.703032318644318,
3.39517483032209));
#11681=CARTESIAN_POINT('Ctrl Pts',(-6.90012184892277,0.893486914765094,
3.41373118314646));
#11682=CARTESIAN_POINT('Ctrl Pts',(-7.39091111614474,0.81012884982552,3.43229760104649));
#11683=CARTESIAN_POINT('Ctrl Pts',(-7.76248245627454,0.478194158159316,
3.45087381180285));
#11684=CARTESIAN_POINT('Ctrl Pts',(-7.87722924504625,0.0791422613117201,
3.4663611170865));
#11685=CARTESIAN_POINT('Ctrl Pts',(-7.83165133922849,-0.240314783834962,
3.47875598768671));
#11686=CARTESIAN_POINT('Ctrl Pts',(-7.70023907701898,-0.535167149935524,
3.49115356884793));
#11687=CARTESIAN_POINT('Ctrl Pts',(-7.39062087111684,-0.812170012694234,
3.50665454205289));
#11688=CARTESIAN_POINT('Ctrl Pts',(-6.89830560717456,-0.896052546468553,
3.52526326778163));
#11689=CARTESIAN_POINT('Ctrl Pts',(-6.48880985910723,-0.725774650674278,
3.54181063235856));
#11690=CARTESIAN_POINT('Ctrl Pts',(-6.24118965329123,-0.437496870629759,
3.55629441767643));
#11691=CARTESIAN_POINT('Ctrl Pts',(-6.13343726805911,-0.130184025345005,
3.5687112475538));
#11692=CARTESIAN_POINT('Ctrl Pts',(-6.14574491655201,0.195411889709324,
3.58113072282879));
#11693=CARTESIAN_POINT('Ctrl Pts',(-6.27593308314913,0.494106501635381,
3.59355230196842));
#11694=CARTESIAN_POINT('Ctrl Pts',(-6.50647484898252,0.72448430278658,3.60597607343073));
#11695=CARTESIAN_POINT('Ctrl Pts',(-6.80518220959668,0.854933539558384,
3.61840163759416));
#11696=CARTESIAN_POINT('Ctrl Pts',(-7.13099645393491,0.867086944731104,
3.6308294909089));
#11697=CARTESIAN_POINT('Ctrl Pts',(-7.37034629814982,0.78331581805002,3.64049644697034));
#11698=CARTESIAN_POINT('Ctrl Pts',(-7.57838611791206,0.645242841704105,
3.65016442339402));
#11699=CARTESIAN_POINT('Ctrl Pts',(-7.77310581402586,0.430433141736348,
3.6612145176939));
#11700=CARTESIAN_POINT('Ctrl Pts',(-7.89226187454386,0.0444204254824345,
3.67640971635602));
#11701=CARTESIAN_POINT('Ctrl Pts',(-7.80129086431032,-0.405895837677021,
3.69367799765519));
#11702=CARTESIAN_POINT('Ctrl Pts',(-7.48064329455355,-0.76503136866683,
3.71163847341778));
#11703=CARTESIAN_POINT('Ctrl Pts',(-6.99989620560288,-0.903501260319285,
3.73029091807058));
#11704=CARTESIAN_POINT('Ctrl Pts',(-6.51931206875194,-0.765010981613905,
3.74894385066014));
#11705=CARTESIAN_POINT('Ctrl Pts',(-6.18598457115065,-0.392062541037647,
3.7675966949923));
#11706=CARTESIAN_POINT('Ctrl Pts',(-6.10224048559192,0.101126455191569,
3.78624875991382));
#11707=CARTESIAN_POINT('Ctrl Pts',(-6.29360664053959,0.563061899641102,
3.80489957562934));
#11708=CARTESIAN_POINT('Ctrl Pts',(-6.70156274884057,0.852798275855841,
3.82354818129352));
#11709=CARTESIAN_POINT('Ctrl Pts',(-7.14516419629844,0.877060146522431,
3.84012284280759));
#11710=CARTESIAN_POINT('Ctrl Pts',(-7.49375117715357,0.724569432080486,
3.85462433846513));
#11711=CARTESIAN_POINT('Ctrl Pts',(-7.72438066713674,0.494215522957976,
3.86705226830291));
#11712=CARTESIAN_POINT('Ctrl Pts',(-7.8546314996621,0.195364139195026,3.87947864210889));
#11713=CARTESIAN_POINT('Ctrl Pts',(-7.86693096726382,-0.130355958792914,
3.89190302709772));
#11714=CARTESIAN_POINT('Ctrl Pts',(-7.75920990140556,-0.437827963480458,
3.90432538766937));
#11715=CARTESIAN_POINT('Ctrl Pts',(-7.54674669970804,-0.685049391800177,
3.91674551833732));
#11716=CARTESIAN_POINT('Ctrl Pts',(-7.2587832470136,-0.836663148820833,
3.92916323122733));
#11717=CARTESIAN_POINT('Ctrl Pts',(-6.82707910403541,-0.886741311123473,
3.94571687930683));
#11718=CARTESIAN_POINT('Ctrl Pts',(-6.31203054929912,-0.639493595762034,
3.966401355575));
#11719=CARTESIAN_POINT('Ctrl Pts',(-6.06084279300897,-0.000449608345310296,
3.99121135126554));
#11720=CARTESIAN_POINT('Ctrl Pts',(-6.31179693592123,0.637682779121499,
4.01600691862606));
#11721=CARTESIAN_POINT('Ctrl Pts',(-6.92918191266279,0.935049780651178,
4.04078798038478));
#11722=CARTESIAN_POINT('Ctrl Pts',(-7.58365238518735,0.732979239453076,
4.06555261138874));
#11723=CARTESIAN_POINT('Ctrl Pts',(-7.9257900806735,0.140447811970743,4.09029979894177));
#11724=CARTESIAN_POINT('Ctrl Pts',(-7.77344406870196,-0.526712992467699,
4.11502804101992));
#11725=CARTESIAN_POINT('Ctrl Pts',(-7.27177779124963,-0.867844577177589,
4.13699100638644));
#11726=CARTESIAN_POINT('Ctrl Pts',(-6.76058665329715,-0.853396344821666,
4.15619430386727));
#11727=CARTESIAN_POINT('Ctrl Pts',(-6.38200074112008,-0.635302741652714,
4.1726443652993));
#11728=CARTESIAN_POINT('Ctrl Pts',(-6.15400141844129,-0.261934603150095,
4.18908432068376));
#11729=CARTESIAN_POINT('Ctrl Pts',(-6.13205747172757,0.174301185046141,
4.20551384069495));
#11730=CARTESIAN_POINT('Ctrl Pts',(-6.32175295930821,0.567698027428144,
4.22193258418429));
#11731=CARTESIAN_POINT('Ctrl Pts',(-6.64654841184092,0.800957389537971,
4.23697195571088));
#11732=CARTESIAN_POINT('Ctrl Pts',(-6.99882766587418,0.867367090001126,
4.25063646985522));
#11733=CARTESIAN_POINT('Ctrl Pts',(-7.31566615380246,0.807532578123425,
4.26292758526584));
#11734=CARTESIAN_POINT('Ctrl Pts',(-7.58839195679831,0.636020296619523,
4.27521192630173));
#11735=CARTESIAN_POINT('Ctrl Pts',(-7.77988431286369,0.37680928883101,4.28748926184605));
#11736=CARTESIAN_POINT('Ctrl Pts',(-7.8626299224257,0.0662152386377366,
4.29975939205125));
#11737=CARTESIAN_POINT('Ctrl Pts',(-7.81589040587151,-0.360959854603563,
4.31611012161726));
#11738=CARTESIAN_POINT('Ctrl Pts',(-7.53509133921148,-0.71291947800451,
4.33244512578823));
#11739=CARTESIAN_POINT('Ctrl Pts',(-7.12976760986697,-0.85322217354558,
4.34876566200336));
#11740=CARTESIAN_POINT('Ctrl Pts',(-6.80953724060416,-0.841669304187541,
4.36099807640831));
#11741=CARTESIAN_POINT('Ctrl Pts',(-6.51549418290265,-0.713177572198111,
4.3732226080825));
#11742=CARTESIAN_POINT('Ctrl Pts',(-6.2888947681933,-0.486688725403999,
4.38543907223306));
#11743=CARTESIAN_POINT('Ctrl Pts',(-6.160920555938,-0.193090427094334,4.39764730462965));
#11744=CARTESIAN_POINT('Ctrl Pts',(-6.14885699254258,0.126741694206413,
4.40984729976258));
#11745=CARTESIAN_POINT('Ctrl Pts',(-6.25465979225549,0.428478434738072,
4.42203873484718));
#11746=CARTESIAN_POINT('Ctrl Pts',(-6.49766240970981,0.711363326767944,
4.43625235165378));
#11747=CARTESIAN_POINT('Ctrl Pts',(-6.89932724358013,0.878345874150377,
4.45248156448681));
#11748=CARTESIAN_POINT('Ctrl Pts',(-7.38168762889607,0.796072531346823,
4.47071928201173));
#11749=CARTESIAN_POINT('Ctrl Pts',(-7.74579952770647,0.470600467593104,
4.48893682127011));
#11750=CARTESIAN_POINT('Ctrl Pts',(-7.88085359657661,0.00163419859513053,
4.50713360807125));
#11751=CARTESIAN_POINT('Ctrl Pts',(-7.74583271530823,-0.466665339744885,
4.52530933877659));
#11752=CARTESIAN_POINT('Ctrl Pts',(-7.38280065073972,-0.791003440257137,
4.54346360414915));
#11753=CARTESIAN_POINT('Ctrl Pts',(-6.90342748857269,-0.872364778276333,
4.56159606648756));
#11754=CARTESIAN_POINT('Ctrl Pts',(-6.45479686015966,-0.686446622036828,
4.57970637146554));
#11755=CARTESIAN_POINT('Ctrl Pts',(-6.17419546746325,-0.290827781409624,
4.59779418863358));
#11756=CARTESIAN_POINT('Ctrl Pts',(-6.14711949228446,0.192830647320786,
4.61585919422455));
#11757=CARTESIAN_POINT('Ctrl Pts',(-6.38122030015602,0.616213166166492,
4.63390107931286));
#11758=CARTESIAN_POINT('Ctrl Pts',(-6.80413193263285,0.849857078671816,
4.65191953970996));
#11759=CARTESIAN_POINT('Ctrl Pts',(-7.28591355768388,0.822695751647876,
4.66991429633147));
#11760=CARTESIAN_POINT('Ctrl Pts',(-7.67882113931455,0.543798193542044,
4.68788504608153));
#11761=CARTESIAN_POINT('Ctrl Pts',(-7.86298344539143,0.0990860698837288,
4.70583158256722));
#11762=CARTESIAN_POINT('Ctrl Pts',(-7.79562977646068,-0.295585883755131,
4.72076651863455));
#11763=CARTESIAN_POINT('Ctrl Pts',(-7.62259402545982,-0.553684972592025,
4.73270226063253));
#11764=CARTESIAN_POINT('Ctrl Pts',(-7.38563136562569,-0.754371890467876,
4.74462971241004));
#11765=CARTESIAN_POINT('Ctrl Pts',(-7.00200477988192,-0.865035088308813,
4.75952323795895));
#11766=CARTESIAN_POINT('Ctrl Pts',(-6.54208755381532,-0.73237927966396,
4.77737036348736));
#11767=CARTESIAN_POINT('Ctrl Pts',(-6.2237590976575,-0.376028323754344,
4.7951920545367));
#11768=CARTESIAN_POINT('Ctrl Pts',(-6.14390675955708,0.0944571090275195,
4.81298816916304));
#11769=CARTESIAN_POINT('Ctrl Pts',(-6.32635880476601,0.534640108883085,
4.83075849956042));
#11770=CARTESIAN_POINT('Ctrl Pts',(-6.71446788666468,0.809896714068275,
4.84850288731427));
#11771=CARTESIAN_POINT('Ctrl Pts',(-7.18884402106963,0.83642032971082,4.86622116373149));
#11772=CARTESIAN_POINT('Ctrl Pts',(-7.6040077565224,0.606854467278431,4.88391319648774));
#11773=CARTESIAN_POINT('Ctrl Pts',(-7.83307416457905,0.192166517804397,
4.90157882330678));
#11774=CARTESIAN_POINT('Ctrl Pts',(-7.80644295598691,-0.280031406976875,
4.91921798059982));
#11775=CARTESIAN_POINT('Ctrl Pts',(-7.53313346814401,-0.665323716801619,
4.93683042576433));
#11776=CARTESIAN_POINT('Ctrl Pts',(-7.0973521810726,-0.845395310573347,
4.95441634803877));
#11777=CARTESIAN_POINT('Ctrl Pts',(-6.63325877718377,-0.76671280820668,
4.97197505561031));
#11778=CARTESIAN_POINT('Ctrl Pts',(-6.28278420709442,-0.453044306679936,
4.98950772058579));
#11779=CARTESIAN_POINT('Ctrl Pts',(-6.19628963467771,-0.152979186566042,
5.00117676314781));
#11780=CARTESIAN_POINT('Ctrl Pts',(-6.19626935608997,-0.00220549038420499,
5.00700843180463));
#11781=CARTESIAN_POINT('Ctrl Pts',(-6.2248547744189,-0.00199943343782885,
1.1016075197803));
#11782=CARTESIAN_POINT('Ctrl Pts',(-6.2248743310293,0.143406873091139,1.10723158692092));
#11783=CARTESIAN_POINT('Ctrl Pts',(-6.30828836165333,0.432372070079823,
1.11847000135813));
#11784=CARTESIAN_POINT('Ctrl Pts',(-6.6449451720994,0.733412609072189,1.13530449261712));
#11785=CARTESIAN_POINT('Ctrl Pts',(-7.08929084993495,0.808561725008331,
1.15211489002863));
#11786=CARTESIAN_POINT('Ctrl Pts',(-7.50521457605639,0.636493535969788,
1.16890177394572));
#11787=CARTESIAN_POINT('Ctrl Pts',(-7.76520183847965,0.269661650219744,
1.18566492040252));
#11788=CARTESIAN_POINT('Ctrl Pts',(-7.79029164728548,-0.178500460126232,
1.20240537393246));
#11789=CARTESIAN_POINT('Ctrl Pts',(-7.5733619556899,-0.570861085094046,
1.21912307461775));
#11790=CARTESIAN_POINT('Ctrl Pts',(-7.1814666343123,-0.787342248857585,
1.23581852081351));
#11791=CARTESIAN_POINT('Ctrl Pts',(-6.73511487871663,-0.762206257537691,
1.25249190232756));
#11792=CARTESIAN_POINT('Ctrl Pts',(-6.37088661927737,-0.503737190939526,
1.26914374509522));
#11793=CARTESIAN_POINT('Ctrl Pts',(-6.22894974433754,-0.160390496771507,
1.28300230726329));
#11794=CARTESIAN_POINT('Ctrl Pts',(-6.23748254588174,0.127860167140178,
1.29407912781801));
#11795=CARTESIAN_POINT('Ctrl Pts',(-6.32460268207204,0.402579634653007,
1.30514903917804));
#11796=CARTESIAN_POINT('Ctrl Pts',(-6.57145353853799,0.679010257848813,
1.31897302616244));
#11797=CARTESIAN_POINT('Ctrl Pts',(-6.99851538436538,0.801913846985834,
1.33554194147043));
#11798=CARTESIAN_POINT('Ctrl Pts',(-7.4248746680664,0.679006428406666,1.35209099258987));
#11799=CARTESIAN_POINT('Ctrl Pts',(-7.72020208132496,0.348444736414998,
1.3686207511464));
#11800=CARTESIAN_POINT('Ctrl Pts',(-7.79428470855507,-0.0880559677436623,
1.38513155285536));
#11801=CARTESIAN_POINT('Ctrl Pts',(-7.62498164492137,-0.496617735919016,
1.40162385464902));
#11802=CARTESIAN_POINT('Ctrl Pts',(-7.26465130631449,-0.752200318832177,
1.41809807629169));
#11803=CARTESIAN_POINT('Ctrl Pts',(-6.82404645473778,-0.776878229830484,
1.43455466287498));
#11804=CARTESIAN_POINT('Ctrl Pts',(-6.43824708026408,-0.563581766788353,
1.45099406485329));
#11805=CARTESIAN_POINT('Ctrl Pts',(-6.22527720772369,-0.178113937475093,
1.46741673691946));
#11806=CARTESIAN_POINT('Ctrl Pts',(-6.25000496641197,0.26114180105586,1.48382315214102));
#11807=CARTESIAN_POINT('Ctrl Pts',(-6.50439363062418,0.619572929497801,
1.50021377495522));
#11808=CARTESIAN_POINT('Ctrl Pts',(-6.91010778310017,0.787561126490409,
1.51658909691877));
#11809=CARTESIAN_POINT('Ctrl Pts',(-7.34261708720444,0.714029319530266,
1.53294958580271));
#11810=CARTESIAN_POINT('Ctrl Pts',(-7.66942871295271,0.421886680885055,
1.54929577826927));
#11811=CARTESIAN_POINT('Ctrl Pts',(-7.79060746309739,0.00107028729058553,
1.56562807006426));
#11812=CARTESIAN_POINT('Ctrl Pts',(-7.66943851128521,-0.419522152665003,
1.58194719524605));
#11813=CARTESIAN_POINT('Ctrl Pts',(-7.39764066575801,-0.662098928380482,
1.59553546104258));
#11814=CARTESIAN_POINT('Ctrl Pts',(-7.12800936410844,-0.747580149118017,
1.60640058684969));
#11815=CARTESIAN_POINT('Ctrl Pts',(-6.84533059531615,-0.75595077651127,
1.61726173262983));
#11816=CARTESIAN_POINT('Ctrl Pts',(-6.52426556122011,-0.622981447977388,
1.6302268277746));
#11817=CARTESIAN_POINT('Ctrl Pts',(-6.28241092024733,-0.303334910575114,
1.64529337928374));
#11818=CARTESIAN_POINT('Ctrl Pts',(-6.22511819857924,0.0766975317585018,
1.65974856169716));
#11819=CARTESIAN_POINT('Ctrl Pts',(-6.35654456974169,0.437774198474303,
1.67419574542797));
#11820=CARTESIAN_POINT('Ctrl Pts',(-6.64450567798582,0.691817599598452,
1.68863515213347));
#11821=CARTESIAN_POINT('Ctrl Pts',(-7.01862615778267,0.777215355234843,
1.7030672564649));
#11822=CARTESIAN_POINT('Ctrl Pts',(-7.3880631251269,0.673250361502341,1.71749234186559));
#11823=CARTESIAN_POINT('Ctrl Pts',(-7.66218237683517,0.405536292432383,
1.73191092401274));
#11824=CARTESIAN_POINT('Ctrl Pts',(-7.78852199146633,-0.00147573673230409,
1.74792521892452));
#11825=CARTESIAN_POINT('Ctrl Pts',(-7.65522108190052,-0.461991819856124,
1.76553253390028));
#11826=CARTESIAN_POINT('Ctrl Pts',(-7.23005076267344,-0.76759871495942,
1.78473130593167));
#11827=CARTESIAN_POINT('Ctrl Pts',(-6.75155429510695,-0.747274686068437,
1.80232278309724));
#11828=CARTESIAN_POINT('Ctrl Pts',(-6.40650202825669,-0.498234630744928,
1.81830900003889));
#11829=CARTESIAN_POINT('Ctrl Pts',(-6.24047280825274,-0.153939971712626,
1.83269297972554));
#11830=CARTESIAN_POINT('Ctrl Pts',(-6.25956175689153,0.228178208148652,
1.84707365028079));
#11831=CARTESIAN_POINT('Ctrl Pts',(-6.45895998733325,0.554399377254544,
1.86145136286506));
#11832=CARTESIAN_POINT('Ctrl Pts',(-6.79000787586996,0.745526894361726,
1.87582668352655));
#11833=CARTESIAN_POINT('Ctrl Pts',(-7.1722480535027,0.755164122979803,1.89019958026226));
#11834=CARTESIAN_POINT('Ctrl Pts',(-7.45546926618143,0.609639094019097,
1.90217609379266));
#11835=CARTESIAN_POINT('Ctrl Pts',(-7.619968516889,0.422826999155373,1.91175692450178));
#11836=CARTESIAN_POINT('Ctrl Pts',(-7.7337590448713,0.201469344983507,1.92133737878384));
#11837=CARTESIAN_POINT('Ctrl Pts',(-7.76555085481583,-0.115361161288046,
1.93331129725923));
#11838=CARTESIAN_POINT('Ctrl Pts',(-7.61724269656214,-0.467517024035713,
1.94768102414047));
#11839=CARTESIAN_POINT('Ctrl Pts',(-7.3184019335958,-0.705892482651842,
1.9620490369602));
#11840=CARTESIAN_POINT('Ctrl Pts',(-6.97345565893835,-0.766400777378709,
1.97522106259225));
#11841=CARTESIAN_POINT('Ctrl Pts',(-6.67002645875538,-0.684883575909834,
1.98719664580064));
#11842=CARTESIAN_POINT('Ctrl Pts',(-6.44246608826879,-0.517098553119758,
1.99797495600939));
#11843=CARTESIAN_POINT('Ctrl Pts',(-6.29209882837185,-0.277608420385701,
2.0087542076441));
#11844=CARTESIAN_POINT('Ctrl Pts',(-6.23942591483951,0.000274968281026084,
2.01953435056931));
#11845=CARTESIAN_POINT('Ctrl Pts',(-6.29209599648858,0.278086990361641,
2.03031566009411));
#11846=CARTESIAN_POINT('Ctrl Pts',(-6.44251218846467,0.517827822733974,
2.04109832171327));
#11847=CARTESIAN_POINT('Ctrl Pts',(-6.67016963267959,0.685306359896662,
2.05188242086643));
#11848=CARTESIAN_POINT('Ctrl Pts',(-7.03460845545162,0.784271696813748,
2.06626368121271));
#11849=CARTESIAN_POINT('Ctrl Pts',(-7.50934705445804,0.638539551533681,
2.08424384481427));
#11850=CARTESIAN_POINT('Ctrl Pts',(-7.80808915927313,0.121217390716024,
2.10582945567952));
#11851=CARTESIAN_POINT('Ctrl Pts',(-7.67515111918521,-0.460869941446203,
2.12742499092525));
#11852=CARTESIAN_POINT('Ctrl Pts',(-7.18151044916999,-0.797599664800736,
2.14903213853423));
#11853=CARTESIAN_POINT('Ctrl Pts',(-6.59025623160929,-0.708519309577169,
2.17065208288646));
#11854=CARTESIAN_POINT('Ctrl Pts',(-6.21717289845826,-0.240812476443051,
2.19228622491967));
#11855=CARTESIAN_POINT('Ctrl Pts',(-6.2618283572727,0.35625085518526,2.21393585669527));
#11856=CARTESIAN_POINT('Ctrl Pts',(-6.70100396959293,0.763867159272458,
2.235602305803));
#11857=CARTESIAN_POINT('Ctrl Pts',(-7.30069183224588,0.763966475773746,
2.25728686433886));
#11858=CARTESIAN_POINT('Ctrl Pts',(-7.74075874128088,0.355786355080811,
2.27899082117545));
#11859=CARTESIAN_POINT('Ctrl Pts',(-7.78576661945122,-0.243320634259026,
2.30071544320844));
#11860=CARTESIAN_POINT('Ctrl Pts',(-7.41089079459932,-0.713588286374201,
2.32246198389553));
#11861=CARTESIAN_POINT('Ctrl Pts',(-6.8155923591716,-0.803439914310088,
2.34423167566847));
#11862=CARTESIAN_POINT('Ctrl Pts',(-6.31753340638779,-0.464026266198107,
2.36602573364463));
#11863=CARTESIAN_POINT('Ctrl Pts',(-6.18312706441087,0.124235781248934,
2.38784535116155));
#11864=CARTESIAN_POINT('Ctrl Pts',(-6.48508519265119,0.647523045910538,
2.40969169944054));
#11865=CARTESIAN_POINT('Ctrl Pts',(-7.06309584210182,0.825972957887767,
2.43156593059124));
#11866=CARTESIAN_POINT('Ctrl Pts',(-7.60891342334618,0.563287329017383,
2.45346916382827));
#11867=CARTESIAN_POINT('Ctrl Pts',(-7.83065866400534,-0.00127617753292936,
2.47540251157));
#11868=CARTESIAN_POINT('Ctrl Pts',(-7.60891844338197,-0.566807923885036,
2.49736702311862));
#11869=CARTESIAN_POINT('Ctrl Pts',(-7.06088009394646,-0.830828943835411,
2.51936379410423));
#11870=CARTESIAN_POINT('Ctrl Pts',(-6.47877456758801,-0.651599257061967,
2.54139372857063));
#11871=CARTESIAN_POINT('Ctrl Pts',(-6.17330829597437,-0.122868357878831,
2.56345805540249));
#11872=CARTESIAN_POINT('Ctrl Pts',(-6.28698448117334,0.372896706566128,
2.5818739530266));
#11873=CARTESIAN_POINT('Ctrl Pts',(-6.56178147714618,0.645909508994359,
2.59662532895527));
#11874=CARTESIAN_POINT('Ctrl Pts',(-6.82755959943639,0.762379250809163,
2.60769790670473));
#11875=CARTESIAN_POINT('Ctrl Pts',(-7.11823191550466,0.77309106288007,2.61877977101866));
#11876=CARTESIAN_POINT('Ctrl Pts',(-7.39283797606485,0.677141608981482,
2.62987102174684));
#11877=CARTESIAN_POINT('Ctrl Pts',(-7.61353492117917,0.487124481673172,
2.64097171794249));
#11878=CARTESIAN_POINT('Ctrl Pts',(-7.74985138987256,0.229489703988864,
2.65208210394633));
#11879=CARTESIAN_POINT('Ctrl Pts',(-7.78235878160371,-0.060347586788017,
2.66320205620807));
#11880=CARTESIAN_POINT('Ctrl Pts',(-7.69452713686875,-0.389520245766072,
2.67618710514898));
#11881=CARTESIAN_POINT('Ctrl Pts',(-7.42968251892112,-0.686854983757288,
2.69104312253098));
#11882=CARTESIAN_POINT('Ctrl Pts',(-6.9981733703996,-0.811041064637613,
2.7077785073907));
#11883=CARTESIAN_POINT('Ctrl Pts',(-6.56643864129979,-0.686766100233019,
2.7245370382011));
#11884=CARTESIAN_POINT('Ctrl Pts',(-6.26644832565199,-0.351246131845318,
2.74131877561319));
#11885=CARTESIAN_POINT('Ctrl Pts',(-6.19089673530764,0.0930086272863596,
2.75812410811431));
#11886=CARTESIAN_POINT('Ctrl Pts',(-6.3635093121898,0.509979233267529,2.77495325162342));
#11887=CARTESIAN_POINT('Ctrl Pts',(-6.73202969542257,0.771572157204226,
2.79180652369004));
#11888=CARTESIAN_POINT('Ctrl Pts',(-7.1839317338843,0.797034153014602,2.80868410758528));
#11889=CARTESIAN_POINT('Ctrl Pts',(-7.58061418049775,0.577885402976202,
2.82558639907399));
#11890=CARTESIAN_POINT('Ctrl Pts',(-7.80043251707909,0.180626646990148,
2.8425133037641));
#11891=CARTESIAN_POINT('Ctrl Pts',(-7.77473827266321,-0.273178159641957,
2.85946578653905));
#11892=CARTESIAN_POINT('Ctrl Pts',(-7.51142930934868,-0.644535621799555,
2.87644320296889));
#11893=CARTESIAN_POINT('Ctrl Pts',(-7.090247475506,-0.819107951266512,2.89344615343804));
#11894=CARTESIAN_POINT('Ctrl Pts',(-6.64007239669075,-0.742719561411661,
2.9104747934985));
#11895=CARTESIAN_POINT('Ctrl Pts',(-6.29901825762491,-0.438060207003031,
2.92752931212875));
#11896=CARTESIAN_POINT('Ctrl Pts',(-6.17213529488574,0.00202864815554152,
2.94460987011375));
#11897=CARTESIAN_POINT('Ctrl Pts',(-6.29903467328276,0.442847147807371,
2.96171662669668));
#11898=CARTESIAN_POINT('Ctrl Pts',(-6.64153900261026,0.749057273900873,
2.97884972234917));
#11899=CARTESIAN_POINT('Ctrl Pts',(-7.09515820674189,0.826230598942998,
2.99600928959219));
#11900=CARTESIAN_POINT('Ctrl Pts',(-7.52096556733847,0.649964042139717,
3.01319544553617));
#11901=CARTESIAN_POINT('Ctrl Pts',(-7.7881416295986,0.273589389598386,3.03040829701253));
#11902=CARTESIAN_POINT('Ctrl Pts',(-7.81416322471417,-0.187958462889913,
3.04764793743321));
#11903=CARTESIAN_POINT('Ctrl Pts',(-7.59029004422625,-0.593236398246943,
3.06491444690837));
#11904=CARTESIAN_POINT('Ctrl Pts',(-7.18447872363049,-0.817636398679871,
3.08220789441772));
#11905=CARTESIAN_POINT('Ctrl Pts',(-6.72075832128736,-0.791696139934339,
3.0995283347252));
#11906=CARTESIAN_POINT('Ctrl Pts',(-6.34132520469639,-0.52259858497262,
3.11687581100324));
#11907=CARTESIAN_POINT('Ctrl Pts',(-6.16294093112047,-0.0922065613935315,
3.13425035266593));
#11908=CARTESIAN_POINT('Ctrl Pts',(-6.24100252329945,0.367838376905317,
3.15165197723848));
#11909=CARTESIAN_POINT('Ctrl Pts',(-6.55234143603862,0.716379447785238,
3.16908068867878));
#11910=CARTESIAN_POINT('Ctrl Pts',(-7.0020918463353,0.846056103485526,3.18653647882978));
#11911=CARTESIAN_POINT('Ctrl Pts',(-7.45259514550158,0.716373955203891,
3.20401932609763));
#11912=CARTESIAN_POINT('Ctrl Pts',(-7.76553445013922,0.366346675369135,
3.22152919662609));
#11913=CARTESIAN_POINT('Ctrl Pts',(-7.84440291089243,-0.0972364168705279,
3.23906604346409));
#11914=CARTESIAN_POINT('Ctrl Pts',(-7.66426531187148,-0.532390368454461,
3.25662980727804));
#11915=CARTESIAN_POINT('Ctrl Pts',(-7.27963605235025,-0.805423137096165,
3.27422041570518));
#11916=CARTESIAN_POINT('Ctrl Pts',(-6.80798248464413,-0.832011638635212,
3.29183778378752));
#11917=CARTESIAN_POINT('Ctrl Pts',(-6.39385226051638,-0.603245168153667,
3.30948181447676));
#11918=CARTESIAN_POINT('Ctrl Pts',(-6.16456258923952,-0.188589753805594,
3.32715239846137));
#11919=CARTESIAN_POINT('Ctrl Pts',(-6.19107396991504,0.285201839732527,
3.34484941106767));
#11920=CARTESIAN_POINT('Ctrl Pts',(-6.46598763617319,0.672844381049206,
3.36257272475332));
#11921=CARTESIAN_POINT('Ctrl Pts',(-6.90568126453254,0.855061730521347,
3.3803221784867));
#11922=CARTESIAN_POINT('Ctrl Pts',(-7.37554004917386,0.775319482500417,
3.39809764885156));
#11923=CARTESIAN_POINT('Ctrl Pts',(-7.7316309447337,0.457299820367578,3.4158988892878));
#11924=CARTESIAN_POINT('Ctrl Pts',(-7.84174000603609,0.0745662310640038,
3.43075473309166));
#11925=CARTESIAN_POINT('Ctrl Pts',(-7.79800365863135,-0.232056476805671,
3.44265191712469));
#11926=CARTESIAN_POINT('Ctrl Pts',(-7.67182066868948,-0.515199447567559,
3.45455755275379));
#11927=CARTESIAN_POINT('Ctrl Pts',(-7.37430850860215,-0.781439283284424,
3.46945566116936));
#11928=CARTESIAN_POINT('Ctrl Pts',(-6.90072597229559,-0.862196711958034,
3.48735835153518));
#11929=CARTESIAN_POINT('Ctrl Pts',(-6.50638111259522,-0.698280648937073,
3.50329380947276));
#11930=CARTESIAN_POINT('Ctrl Pts',(-6.26771696466849,-0.420467232665984,
3.51725294127665));
#11931=CARTESIAN_POINT('Ctrl Pts',(-6.16378327673368,-0.124090742239312,
3.52922891646493));
#11932=CARTESIAN_POINT('Ctrl Pts',(-6.17563970316166,0.190145148682862,
3.541215543978));
#11933=CARTESIAN_POINT('Ctrl Pts',(-6.30136031675994,0.47862813180961,3.5532129233572));
#11934=CARTESIAN_POINT('Ctrl Pts',(-6.52415787063659,0.701300976048231,
3.5652208283079));
#11935=CARTESIAN_POINT('Ctrl Pts',(-6.81305446865538,0.827485478120808,
3.57723931168856));
#11936=CARTESIAN_POINT('Ctrl Pts',(-7.12839417303149,0.839273074556283,
3.58926795489742));
#11937=CARTESIAN_POINT('Ctrl Pts',(-7.36023102178962,0.758149247707102,
3.59863178178537));
#11938=CARTESIAN_POINT('Ctrl Pts',(-7.5618318245833,0.624353944762267,3.60800077373871));
#11939=CARTESIAN_POINT('Ctrl Pts',(-7.75062769361495,0.416108732983249,
3.61871415916585));
#11940=CARTESIAN_POINT('Ctrl Pts',(-7.86629928772947,0.0415532963064746,
3.63345965175506));
#11941=CARTESIAN_POINT('Ctrl Pts',(-7.7779918817253,-0.39587268229449,3.65023477657817));
#11942=CARTESIAN_POINT('Ctrl Pts',(-7.46625718079828,-0.745141782522388,
3.66770107275509));
#11943=CARTESIAN_POINT('Ctrl Pts',(-6.99827607275313,-0.88002130153468,
3.68586089589016));
#11944=CARTESIAN_POINT('Ctrl Pts',(-6.52986865734608,-0.745124581336043,
3.70404217195174));
#11945=CARTESIAN_POINT('Ctrl Pts',(-6.20456394041314,-0.381273654072062,
3.7222445238637));
#11946=CARTESIAN_POINT('Ctrl Pts',(-6.12267644558823,0.100510595544224,
3.74046764828387));
#11947=CARTESIAN_POINT('Ctrl Pts',(-6.30977183326723,0.552341449898111,
3.75871108111533));
#11948=CARTESIAN_POINT('Ctrl Pts',(-6.70921301060823,0.836129267279029,
3.77697467535039));
#11949=CARTESIAN_POINT('Ctrl Pts',(-7.1441245198916,0.859984988516024,3.79322614015507));
#11950=CARTESIAN_POINT('Ctrl Pts',(-7.48623548722456,0.710359638299156,
3.80745809953178));
#11951=CARTESIAN_POINT('Ctrl Pts',(-7.71277070102754,0.48412224747983,3.81966559227767));
#11952=CARTESIAN_POINT('Ctrl Pts',(-7.84083027759801,0.190364482880831,
3.83188120516031));
#11953=CARTESIAN_POINT('Ctrl Pts',(-7.85295030253414,-0.130075942851775,
3.84410504587178));
#11954=CARTESIAN_POINT('Ctrl Pts',(-7.74691363433699,-0.43282273789263,
3.85633683595988));
#11955=CARTESIAN_POINT('Ctrl Pts',(-7.53756814795209,-0.676450487908387,
3.86857651327384));
#11956=CARTESIAN_POINT('Ctrl Pts',(-7.25358196284646,-0.825999495253873,
3.8808239163173));
#11957=CARTESIAN_POINT('Ctrl Pts',(-6.82749009436362,-0.875459457105686,
3.8971638473309));
#11958=CARTESIAN_POINT('Ctrl Pts',(-6.31840599454854,-0.631272784946072,
3.91760800377417));
#11959=CARTESIAN_POINT('Ctrl Pts',(-6.06955728718615,0.00123803732983087,
3.94216897705183));
#11960=CARTESIAN_POINT('Ctrl Pts',(-6.31819102434332,0.634074482232743,
3.96675822887569));
#11961=CARTESIAN_POINT('Ctrl Pts',(-6.9313053376154,0.929622791355819,3.99137353813945));
#11962=CARTESIAN_POINT('Ctrl Pts',(-7.58250506298981,0.728789845168479,
4.01601424493145));
#11963=CARTESIAN_POINT('Ctrl Pts',(-7.92366256220496,0.138392594622019,
4.04067889340962));
#11964=CARTESIAN_POINT('Ctrl Pts',(-7.77179568222589,-0.527662971229173,
4.06536647515298));
#11965=CARTESIAN_POINT('Ctrl Pts',(-7.27025795697357,-0.868934722949909,
4.08732996841401));
#11966=CARTESIAN_POINT('Ctrl Pts',(-6.75835124126733,-0.854544547073557,
4.10656171053866));
#11967=CARTESIAN_POINT('Ctrl Pts',(-6.37879399711334,-0.635954794669273,
4.1230547880809));
#11968=CARTESIAN_POINT('Ctrl Pts',(-6.1499093463627,-0.261266758101386,
4.13955596485591));
#11969=CARTESIAN_POINT('Ctrl Pts',(-6.12780704819221,0.177035632837681,
4.15606488283879));
#11970=CARTESIAN_POINT('Ctrl Pts',(-6.31855578375345,0.572773125836556,
4.17258104025126));
#11971=CARTESIAN_POINT('Ctrl Pts',(-6.64561065324521,0.807715171173621,
4.18772845995009));
#11972=CARTESIAN_POINT('Ctrl Pts',(-7.00069569962751,0.87468645863181,4.20150256960693));
#11973=CARTESIAN_POINT('Ctrl Pts',(-7.32033825743143,0.814344340487275,
4.21390324929584));
#11974=CARTESIAN_POINT('Ctrl Pts',(-7.59571864682914,0.641195296318534,
4.22630725980721));
#11975=CARTESIAN_POINT('Ctrl Pts',(-7.78924451820651,0.379269985559648,
4.23871461172216));
#11976=CARTESIAN_POINT('Ctrl Pts',(-7.87295367538825,0.0651494056917473,
4.25112517528242));
#11977=CARTESIAN_POINT('Ctrl Pts',(-7.82568225268596,-0.367234171521722,
4.26767616713046));
#11978=CARTESIAN_POINT('Ctrl Pts',(-7.54119300812834,-0.724025248548577,
4.28423413721587));
#11979=CARTESIAN_POINT('Ctrl Pts',(-7.1299107823301,-0.866436168146,4.30079557699508));
#11980=CARTESIAN_POINT('Ctrl Pts',(-6.80469982154594,-0.854722697198128,
4.31321922941577));
#11981=CARTESIAN_POINT('Ctrl Pts',(-6.50582530202995,-0.724153314531107,
4.32564485900137));
#11982=CARTESIAN_POINT('Ctrl Pts',(-6.27530903670794,-0.493779918883838,
4.3380724340676));
#11983=CARTESIAN_POINT('Ctrl Pts',(-6.14499807654234,-0.194895279444064,
4.35050178414795));
#11984=CARTESIAN_POINT('Ctrl Pts',(-6.1326836203633,0.130969847315759,4.36293259153097));
#11985=CARTESIAN_POINT('Ctrl Pts',(-6.24054332790336,0.438658395770793,
4.37536497831168));
#11986=CARTESIAN_POINT('Ctrl Pts',(-6.48850361176595,0.727358100762058,
4.38987036538262));
#11987=CARTESIAN_POINT('Ctrl Pts',(-6.89878519788956,0.898005260436416,
4.40645053432791));
#11988=CARTESIAN_POINT('Ctrl Pts',(-7.39214301970602,0.81394727492655,4.42510540352934));
#11989=CARTESIAN_POINT('Ctrl Pts',(-7.7650364742413,0.480739139420634,4.44376113789487));
#11990=CARTESIAN_POINT('Ctrl Pts',(-7.90357160220274,-3.623103406608E-6,
4.46241753166182));
#11991=CARTESIAN_POINT('Ctrl Pts',(-7.765072064783,-0.48066867355125,4.48107386788255));
#11992=CARTESIAN_POINT('Ctrl Pts',(-7.39209692797424,-0.813999851714318,
4.49972963764179));
#11993=CARTESIAN_POINT('Ctrl Pts',(-6.89897204270138,-0.897777064686935,
4.51838423828675));
#11994=CARTESIAN_POINT('Ctrl Pts',(-6.43690579425127,-0.706377273901182,
4.53703710208272));
#11995=CARTESIAN_POINT('Ctrl Pts',(-6.14753182130078,-0.29852635300287,
4.55568763786335));
#11996=CARTESIAN_POINT('Ctrl Pts',(-6.11950670544268,0.200690311117515,
4.57433527397971));
#11997=CARTESIAN_POINT('Ctrl Pts',(-6.36133752232976,0.638212076438947,
4.59297941498749));
#11998=CARTESIAN_POINT('Ctrl Pts',(-6.79877170304226,0.879965848122953,
4.6116195104013));
#11999=CARTESIAN_POINT('Ctrl Pts',(-7.29767685928348,0.851914437330659,
4.63025492201343));
#12000=CARTESIAN_POINT('Ctrl Pts',(-7.70501759766691,0.562861344844633,
4.64888520633693));
#12001=CARTESIAN_POINT('Ctrl Pts',(-7.89619288084634,0.101410721742439,
4.66750951337591));
#12002=CARTESIAN_POINT('Ctrl Pts',(-7.82628685314434,-0.308577267495686,
4.68302485728523));
#12003=CARTESIAN_POINT('Ctrl Pts',(-7.64641803457992,-0.576889867652478,
4.69543289868442));
#12004=CARTESIAN_POINT('Ctrl Pts',(-7.39997233303158,-0.785623378939254,
4.7078385298175));
#12005=CARTESIAN_POINT('Ctrl Pts',(-7.00068720444936,-0.900862697549362,
4.72334181510526));
#12006=CARTESIAN_POINT('Ctrl Pts',(-6.52149454897357,-0.762718702390436,
4.74193719606482));
#12007=CARTESIAN_POINT('Ctrl Pts',(-6.18946749999406,-0.391136044010536,
4.76052410820248));
#12008=CARTESIAN_POINT('Ctrl Pts',(-6.1060469913375,0.0999708129477241,
4.77910172767096));
#12009=CARTESIAN_POINT('Ctrl Pts',(-6.29661517993785,0.559908233001406,
4.79766964181958));
#12010=CARTESIAN_POINT('Ctrl Pts',(-6.70244964702483,0.847815493498755,
4.81622723951419));
#12011=CARTESIAN_POINT('Ctrl Pts',(-7.19897393950221,0.875640964323189,
4.83477405165335));
#12012=CARTESIAN_POINT('Ctrl Pts',(-7.63393210347268,0.635199165297035,
4.85330946175398));
#12013=CARTESIAN_POINT('Ctrl Pts',(-7.87415840450806,0.200428618681077,
4.87183314873462));
#12014=CARTESIAN_POINT('Ctrl Pts',(-7.8462682157887,-0.295087980091751,
4.89034419343159));
#12015=CARTESIAN_POINT('Ctrl Pts',(-7.559270479536,-0.6997578181279,4.90884305096593));
#12016=CARTESIAN_POINT('Ctrl Pts',(-7.10125854846447,-0.889082640532772,
4.9273272036816));
#12017=CARTESIAN_POINT('Ctrl Pts',(-6.61308396712537,-0.806345361743623,
4.94579808431053));
#12018=CARTESIAN_POINT('Ctrl Pts',(-6.24411722187037,-0.47624035230175,
4.96425287782899));
#12019=CARTESIAN_POINT('Ctrl Pts',(-6.15296011813682,-0.160062489926647,
4.97654946949845));
#12020=CARTESIAN_POINT('Ctrl Pts',(-6.15293876115034,-0.00127077166344464,
4.98269126153386));
#12021=CARTESIAN_POINT('Ctrl Pts',(-6.17520256096103,-0.00198708894523262,
1.10146101760312));
#12022=CARTESIAN_POINT('Ctrl Pts',(-6.17522335720648,0.152636088641731,
1.10744157754584));
#12023=CARTESIAN_POINT('Ctrl Pts',(-6.26397421604634,0.460181465931467,
1.11940264078387));
#12024=CARTESIAN_POINT('Ctrl Pts',(-6.62219829265502,0.780474598552503,
1.13731436110618));
#12025=CARTESIAN_POINT('Ctrl Pts',(-7.09502710563339,0.8604640532775,1.15520328301464));
#12026=CARTESIAN_POINT('Ctrl Pts',(-7.53761123589857,0.677356597316656,
1.17306606520991));
#12027=CARTESIAN_POINT('Ctrl Pts',(-7.81425257067584,0.287026630697464,
1.19090382222027));
#12028=CARTESIAN_POINT('Ctrl Pts',(-7.84094181593244,-0.189822561848461,
1.20871600217045));
#12029=CARTESIAN_POINT('Ctrl Pts',(-7.61013966093306,-0.607254329738822,
1.22650257068965));
#12030=CARTESIAN_POINT('Ctrl Pts',(-7.19324067176169,-0.837535007289599,
1.24426328742192));
#12031=CARTESIAN_POINT('Ctrl Pts',(-6.71848758862675,-0.81078612394349,
1.26199799446351));
#12032=CARTESIAN_POINT('Ctrl Pts',(-6.33116022346325,-0.535907604875262,
1.2797065735325));
#12033=CARTESIAN_POINT('Ctrl Pts',(-6.18026207378729,-0.170848153165099,
1.29444173805585));
#12034=CARTESIAN_POINT('Ctrl Pts',(-6.18933579538129,0.135568276904099,
1.3062167913918));
#12035=CARTESIAN_POINT('Ctrl Pts',(-6.28193796907153,0.427563933921057,
1.31798301358477));
#12036=CARTESIAN_POINT('Ctrl Pts',(-6.5442756777705,0.721311430477084,1.33267407278365));
#12037=CARTESIAN_POINT('Ctrl Pts',(-6.99797673974231,0.85185791707026,1.35027676526993));
#12038=CARTESIAN_POINT('Ctrl Pts',(-7.45077008597338,0.72130574984839,1.36785270105323));
#12039=CARTESIAN_POINT('Ctrl Pts',(-7.76428017317448,0.370353167602943,
1.38540183844591));
#12040=CARTESIAN_POINT('Ctrl Pts',(-7.84287078731736,-0.0928749009693313,
1.40292409570255));
#12041=CARTESIAN_POINT('Ctrl Pts',(-7.66325053119436,-0.526256204532712,
1.42041942701044));
#12042=CARTESIAN_POINT('Ctrl Pts',(-7.28117348427495,-0.797224750052114,
1.43788778901988));
#12043=CARTESIAN_POINT('Ctrl Pts',(-6.81422094277963,-0.823344619257912,
1.45532915596481));
#12044=CARTESIAN_POINT('Ctrl Pts',(-6.40557740007369,-0.597377670958505,
1.47274351267088));
#12045=CARTESIAN_POINT('Ctrl Pts',(-6.18014135114604,-0.189269109963645,
1.49013085807296));
#12046=CARTESIAN_POINT('Ctrl Pts',(-6.2063447813037,0.275500641446163,1.50749120271993));
#12047=CARTESIAN_POINT('Ctrl Pts',(-6.47538428641671,0.654503435576307,
1.52482457231741));
#12048=CARTESIAN_POINT('Ctrl Pts',(-6.90415993114079,0.831993637590178,
1.54213100041399));
#12049=CARTESIAN_POINT('Ctrl Pts',(-7.36093058729913,0.754291131752931,
1.55941054503198));
#12050=CARTESIAN_POINT('Ctrl Pts',(-7.70581436675896,0.445930495584409,
1.57666325226967));
#12051=CARTESIAN_POINT('Ctrl Pts',(-7.83356805338808,0.00210351736980688,
1.59388923591928));
#12052=CARTESIAN_POINT('Ctrl Pts',(-7.70582394465435,-0.441132803023751,
1.61108850297208));
#12053=CARTESIAN_POINT('Ctrl Pts',(-7.41957271786401,-0.696552747164017,
1.6253992073661));
#12054=CARTESIAN_POINT('Ctrl Pts',(-7.13580562433151,-0.786506150070278,
1.63683431952564));
#12055=CARTESIAN_POINT('Ctrl Pts',(-6.83842565990734,-0.795302935598094,
1.64826062329981));
#12056=CARTESIAN_POINT('Ctrl Pts',(-6.50087883949155,-0.655459856237676,
1.66189334009304));
#12057=CARTESIAN_POINT('Ctrl Pts',(-6.24683856091248,-0.319636583957497,
1.67772217495051));
#12058=CARTESIAN_POINT('Ctrl Pts',(-6.18673593956685,0.0792979977372244,
1.6928973583662));
#12059=CARTESIAN_POINT('Ctrl Pts',(-6.32462763406589,0.458013354632876,
1.70805202838354));
#12060=CARTESIAN_POINT('Ctrl Pts',(-6.6264499004516,0.724227994182597,1.72318637191565));
#12061=CARTESIAN_POINT('Ctrl Pts',(-7.01822731079915,0.813611152577389,
1.73830047742657));
#12062=CARTESIAN_POINT('Ctrl Pts',(-7.40474814051684,0.704789757388159,
1.75339453601228));
#12063=CARTESIAN_POINT('Ctrl Pts',(-7.69127468028525,0.424899737053255,
1.76846861925216));
#12064=CARTESIAN_POINT('Ctrl Pts',(-7.82317524134296,-0.000214256054242891,
1.78519536337412));
#12065=CARTESIAN_POINT('Ctrl Pts',(-7.68400292544061,-0.480657578694496,
1.80356687214843));
#12066=CARTESIAN_POINT('Ctrl Pts',(-7.24089307934962,-0.799010630883542,
1.82357396776757));
#12067=CARTESIAN_POINT('Ctrl Pts',(-6.74293367382506,-0.777755869248963,
1.84188239224313));
#12068=CARTESIAN_POINT('Ctrl Pts',(-6.38428160300257,-0.518827919852002,
1.8585022780832));
#12069=CARTESIAN_POINT('Ctrl Pts',(-6.21190652336758,-0.161263271843629,
1.87344136056984));
#12070=CARTESIAN_POINT('Ctrl Pts',(-6.23176145956434,0.235155052909281,
1.88836189008528));
#12071=CARTESIAN_POINT('Ctrl Pts',(-6.43845468102026,0.573210094242605,
1.90326411778669));
#12072=CARTESIAN_POINT('Ctrl Pts',(-6.78120758623466,0.771036152968419,
1.91814814537143));
#12073=CARTESIAN_POINT('Ctrl Pts',(-7.17651986260646,0.780947526175952,
1.93301451057625));
#12074=CARTESIAN_POINT('Ctrl Pts',(-7.4690838087241,0.6305742769914,1.94538806622837));
#12075=CARTESIAN_POINT('Ctrl Pts',(-7.63887158061852,0.43774021307995,1.95527801683068));
#12076=CARTESIAN_POINT('Ctrl Pts',(-7.75625455717709,0.209372765981586,
1.96516220579056));
#12077=CARTESIAN_POINT('Ctrl Pts',(-7.78897772922025,-0.117235198065406,
1.97750752002541));
#12078=CARTESIAN_POINT('Ctrl Pts',(-7.63621849985398,-0.479805178484218,
1.99230385729475));
#12079=CARTESIAN_POINT('Ctrl Pts',(-7.3288106015314,-0.724940155926844,
2.00708477487171));
#12080=CARTESIAN_POINT('Ctrl Pts',(-6.97443057853455,-0.787047878698219,
2.02061813346151));
#12081=CARTESIAN_POINT('Ctrl Pts',(-6.663036910551,-0.703366340083497,2.03290903791219));
#12082=CARTESIAN_POINT('Ctrl Pts',(-6.429713249652,-0.531296785721741,2.04396215844239));
#12083=CARTESIAN_POINT('Ctrl Pts',(-6.27568069467376,-0.285929863314846,
2.05500628203848));
#12084=CARTESIAN_POINT('Ctrl Pts',(-6.22179379652821,-0.00148447165528299,
2.06604174225271));
#12085=CARTESIAN_POINT('Ctrl Pts',(-6.27567723842726,0.282625283926166,
2.0770685423675));
#12086=CARTESIAN_POINT('Ctrl Pts',(-6.42939321834636,0.527569244817696,
2.08808682846216));
#12087=CARTESIAN_POINT('Ctrl Pts',(-6.66180436480139,0.698523534700444,
2.09909676470742));
#12088=CARTESIAN_POINT('Ctrl Pts',(-7.03352012631891,0.799423308390042,
2.11376548571774));
#12089=CARTESIAN_POINT('Ctrl Pts',(-7.51702000256108,0.650830743926028,
2.13208194275696));
#12090=CARTESIAN_POINT('Ctrl Pts',(-7.8205544699971,0.12477872778957,2.15402963008721));
#12091=CARTESIAN_POINT('Ctrl Pts',(-7.68544758554438,-0.465859683502365,
2.17594706678624));
#12092=CARTESIAN_POINT('Ctrl Pts',(-7.18532832918539,-0.806749907827285,
2.19783506274917));
#12093=CARTESIAN_POINT('Ctrl Pts',(-6.58761900266066,-0.716477849063796,
2.21969487371389));
#12094=CARTESIAN_POINT('Ctrl Pts',(-6.21132525852498,-0.244398599379355,
2.24152759150295));
#12095=CARTESIAN_POINT('Ctrl Pts',(-6.2565166557362,0.3569122874933,2.26333440391098));
#12096=CARTESIAN_POINT('Ctrl Pts',(-6.69813227966462,0.766495972123007,
2.2851164884739));
#12097=CARTESIAN_POINT('Ctrl Pts',(-7.29979559743913,0.766377681005144,
2.30687505361852));
#12098=CARTESIAN_POINT('Ctrl Pts',(-7.7403172038414,0.357478557881761,2.32861132352834));
#12099=CARTESIAN_POINT('Ctrl Pts',(-7.78508314321668,-0.241314211311507,
2.35032654112574));
#12100=CARTESIAN_POINT('Ctrl Pts',(-7.41096299128847,-0.710285258646494,
2.37202196782575));
#12101=CARTESIAN_POINT('Ctrl Pts',(-6.81823980426185,-0.799529018877506,
2.39369887989847));
#12102=CARTESIAN_POINT('Ctrl Pts',(-6.32343193216603,-0.462069625636124,
2.41535857127149));
#12103=CARTESIAN_POINT('Ctrl Pts',(-6.19033403334486,0.121430361598332,
2.43700234837564));
#12104=CARTESIAN_POINT('Ctrl Pts',(-6.48944013553029,0.639347819738511,
2.45863153303831));
#12105=CARTESIAN_POINT('Ctrl Pts',(-7.06062039853485,0.815467008999971,
2.48024745795251));
#12106=CARTESIAN_POINT('Ctrl Pts',(-7.59882665791512,0.556211166886447,
2.50185147160134));
#12107=CARTESIAN_POINT('Ctrl Pts',(-7.81691597971047,0.00038587243355178,
2.52344492141857));
#12108=CARTESIAN_POINT('Ctrl Pts',(-7.59884810631217,-0.555213231600651,
2.5450292014295));
#12109=CARTESIAN_POINT('Ctrl Pts',(-7.06125744429576,-0.813974168132374,
2.56660562283359));
#12110=CARTESIAN_POINT('Ctrl Pts',(-6.49143383198293,-0.638312378386942,
2.58817573968482));
#12111=CARTESIAN_POINT('Ctrl Pts',(-6.19309159486605,-0.121506544825599,
2.60974057380503));
#12112=CARTESIAN_POINT('Ctrl Pts',(-6.30414628890434,0.362095563250968,
2.62770881360045));
#12113=CARTESIAN_POINT('Ctrl Pts',(-6.57188215917242,0.628050171743863,
2.64208135096746));
#12114=CARTESIAN_POINT('Ctrl Pts',(-6.83060733093959,0.741402467988298,
2.65286053512832));
#12115=CARTESIAN_POINT('Ctrl Pts',(-7.11331019485116,0.751800822313028,
2.66363943998543));
#12116=CARTESIAN_POINT('Ctrl Pts',(-7.38015321254041,0.658536578249394,
2.67441829878632));
#12117=CARTESIAN_POINT('Ctrl Pts',(-7.59442540813206,0.474028701024785,
2.68519731735848));
#12118=CARTESIAN_POINT('Ctrl Pts',(-7.72664835318823,0.224078813661572,
2.69597649059435));
#12119=CARTESIAN_POINT('Ctrl Pts',(-7.75814251512839,-0.0568684122326128,
2.7067563322709));
#12120=CARTESIAN_POINT('Ctrl Pts',(-7.67305026831101,-0.375670601170515,
2.71933299465532));
#12121=CARTESIAN_POINT('Ctrl Pts',(-7.41675242429056,-0.663319154262185,
2.73370861079294));
#12122=CARTESIAN_POINT('Ctrl Pts',(-6.99972126318494,-0.783265764622907,
2.74988403280801));
#12123=CARTESIAN_POINT('Ctrl Pts',(-6.58300990508826,-0.663244925260623,
2.76606207030967));
#12124=CARTESIAN_POINT('Ctrl Pts',(-6.29383153821051,-0.339717208918772,
2.78224374459041));
#12125=CARTESIAN_POINT('Ctrl Pts',(-6.22114054700406,0.0881212098583566,
2.79842947681081));
#12126=CARTESIAN_POINT('Ctrl Pts',(-6.38724602124502,0.489197356400545,
2.81461997314655));
#12127=CARTESIAN_POINT('Ctrl Pts',(-6.74139139837251,0.740504683130387,
2.83081572177923));
#12128=CARTESIAN_POINT('Ctrl Pts',(-7.17515482616827,0.76487797258106,2.84701748262569));
#12129=CARTESIAN_POINT('Ctrl Pts',(-7.55548063740019,0.554694931751024,
2.86322547779102));
#12130=CARTESIAN_POINT('Ctrl Pts',(-7.76598006770104,0.174143761765996,
2.87944106971308));
#12131=CARTESIAN_POINT('Ctrl Pts',(-7.74133660602088,-0.260082341241471,
2.89566309355239));
#12132=CARTESIAN_POINT('Ctrl Pts',(-7.48957685241318,-0.615046118600353,
2.91189415966483));
#12133=CARTESIAN_POINT('Ctrl Pts',(-7.08731533016645,-0.781714319571146,
2.92813385307331));
#12134=CARTESIAN_POINT('Ctrl Pts',(-6.65779777358391,-0.70877510401241,
2.94438283541206));
#12135=CARTESIAN_POINT('Ctrl Pts',(-6.33271975622983,-0.418314727228539,
2.96064163431084));
#12136=CARTESIAN_POINT('Ctrl Pts',(-6.21192448996774,0.000848146316009892,
2.97691080417122));
#12137=CARTESIAN_POINT('Ctrl Pts',(-6.33273084797174,0.420316475281392,
2.99319088962537));
#12138=CARTESIAN_POINT('Ctrl Pts',(-6.65841919119061,0.711426102093092,
3.00948242360202));
#12139=CARTESIAN_POINT('Ctrl Pts',(-7.08938365463165,0.78469653047417,3.02578593995235));
#12140=CARTESIAN_POINT('Ctrl Pts',(-7.49358481171723,0.61732386108425,3.04210195971773));
#12141=CARTESIAN_POINT('Ctrl Pts',(-7.74698795349186,0.260274136600851,
3.05843100290411));
#12142=CARTESIAN_POINT('Ctrl Pts',(-7.77161091961628,-0.177229268565413,
3.07477358371368));
#12143=CARTESIAN_POINT('Ctrl Pts',(-7.5595133072481,-0.561104620871015,
3.0911302014686));
#12144=CARTESIAN_POINT('Ctrl Pts',(-7.17535047001025,-0.773488637585987,
3.10750136160667));
#12145=CARTESIAN_POINT('Ctrl Pts',(-6.73667244369075,-0.748911461799866,
3.12388755084162));
#12146=CARTESIAN_POINT('Ctrl Pts',(-6.3779682885093,-0.494471004158721,
3.14028925748387));
#12147=CARTESIAN_POINT('Ctrl Pts',(-6.20944935172518,-0.0877920636709064,
3.15670695538732));
#12148=CARTESIAN_POINT('Ctrl Pts',(-6.28319879502128,0.346646282224702,
3.17314111625288));
#12149=CARTESIAN_POINT('Ctrl Pts',(-6.57708076320731,0.675598555420789,
3.18959220330918));
#12150=CARTESIAN_POINT('Ctrl Pts',(-7.00137860324948,0.797906523574267,
3.20606066596027));
#12151=CARTESIAN_POINT('Ctrl Pts',(-7.42617378260305,0.675596701009556,
3.22254695486609));
#12152=CARTESIAN_POINT('Ctrl Pts',(-7.72111320507981,0.345664903192319,
3.23905150388902));
#12153=CARTESIAN_POINT('Ctrl Pts',(-7.7953969119236,-0.0911079815633575,
3.25557474416723));
#12154=CARTESIAN_POINT('Ctrl Pts',(-7.62572261395765,-0.500930075649132,
3.27211709319075));
#12155=CARTESIAN_POINT('Ctrl Pts',(-7.26359060619952,-0.757969018039986,
3.28867896364162));
#12156=CARTESIAN_POINT('Ctrl Pts',(-6.8196773785154,-0.782976033006322,
3.3052607585784));
#12157=CARTESIAN_POINT('Ctrl Pts',(-6.43002407375901,-0.567712626192564,
3.32186286665882));
#12158=CARTESIAN_POINT('Ctrl Pts',(-6.2143495238102,-0.177650477030896,
3.33848567746599));
#12159=CARTESIAN_POINT('Ctrl Pts',(-6.23929452274523,0.267931676361288,
3.35512955696615));
#12160=CARTESIAN_POINT('Ctrl Pts',(-6.4977981727106,0.632417428400449,3.3717948862143));
#12161=CARTESIAN_POINT('Ctrl Pts',(-6.91116723721851,0.803716352677741,
3.38848198687104));
#12162=CARTESIAN_POINT('Ctrl Pts',(-7.35283140859241,0.728752415779589,
3.40519128182654));
#12163=CARTESIAN_POINT('Ctrl Pts',(-7.68751682991823,0.429843740878194,
3.42192294577688));
#12164=CARTESIAN_POINT('Ctrl Pts',(-7.79099865641625,0.0701396538138709,
3.43588523419587));
#12165=CARTESIAN_POINT('Ctrl Pts',(-7.74989579680847,-0.21802096983869,
3.44706617600471));
#12166=CARTESIAN_POINT('Ctrl Pts',(-7.63131205058786,-0.48411169588832,
3.45825488852589));
#12167=CARTESIAN_POINT('Ctrl Pts',(-7.35171966125215,-0.734316353658553,
3.47225592024697));
#12168=CARTESIAN_POINT('Ctrl Pts',(-6.90665634422983,-0.810213610247401,
3.48908075059773));
#12169=CARTESIAN_POINT('Ctrl Pts',(-6.53604125268008,-0.656166268075892,
3.50405734901444));
#12170=CARTESIAN_POINT('Ctrl Pts',(-6.31172510564101,-0.395058130413869,
3.51717721810318));
#12171=CARTESIAN_POINT('Ctrl Pts',(-6.21403211052705,-0.11648505246751,
3.5284338585998));
#12172=CARTESIAN_POINT('Ctrl Pts',(-6.22517418787314,0.178897331422162,
3.53970134734807));
#12173=CARTESIAN_POINT('Ctrl Pts',(-6.34335895664989,0.450096638989748,
3.55097987580857));
#12174=CARTESIAN_POINT('Ctrl Pts',(-6.55282538255646,0.659451018575483,
3.56226945063314));
#12175=CARTESIAN_POINT('Ctrl Pts',(-6.82446778576932,0.778103756403872,
3.57357018144722));
#12176=CARTESIAN_POINT('Ctrl Pts',(-7.12101306693323,0.789192713545858,
3.58488192569325));
#12177=CARTESIAN_POINT('Ctrl Pts',(-7.33906330667987,0.712896965876082,
3.59368882725176));
#12178=CARTESIAN_POINT('Ctrl Pts',(-7.52869402188939,0.58704644286916,3.60250150300269));
#12179=CARTESIAN_POINT('Ctrl Pts',(-7.70630123965848,0.391148862353906,
3.61257978479708));
#12180=CARTESIAN_POINT('Ctrl Pts',(-7.81514745185466,0.0387319382513335,
3.62645378552755));
#12181=CARTESIAN_POINT('Ctrl Pts',(-7.7320534206871,-0.372945464851778,
3.64224111773929));
#12182=CARTESIAN_POINT('Ctrl Pts',(-7.43860263654834,-0.701759159899474,
3.65868352683148));
#12183=CARTESIAN_POINT('Ctrl Pts',(-6.99790910892847,-0.828797861504417,
3.67578437922259));
#12184=CARTESIAN_POINT('Ctrl Pts',(-6.55664423613565,-0.70174357995305,
3.69291144840077));
#12185=CARTESIAN_POINT('Ctrl Pts',(-6.25005791143385,-0.358869278941272,
3.7100648670323));
#12186=CARTESIAN_POINT('Ctrl Pts',(-6.17282669341117,0.0953431157116756,
3.72724477239473));
#12187=CARTESIAN_POINT('Ctrl Pts',(-6.34926472763597,0.521516954352712,
3.74445126049261));
#12188=CARTESIAN_POINT('Ctrl Pts',(-6.72616431631433,0.789332181942143,
3.76168447228502));
#12189=CARTESIAN_POINT('Ctrl Pts',(-7.13675574522559,0.811884513458825,
3.77702664030951));
#12190=CARTESIAN_POINT('Ctrl Pts',(-7.45988117366292,0.670575550442469,
3.79046840933465));
#12191=CARTESIAN_POINT('Ctrl Pts',(-7.67392353281915,0.456831908457597,
3.80200188063455));
#12192=CARTESIAN_POINT('Ctrl Pts',(-7.79496970644638,0.179188233396773,
3.81354733579817));
#12193=CARTESIAN_POINT('Ctrl Pts',(-7.80644272472456,-0.12379090386609,
3.8251047492067));
#12194=CARTESIAN_POINT('Ctrl Pts',(-7.70615482539854,-0.410154530705009,
3.83667418041178));
#12195=CARTESIAN_POINT('Ctrl Pts',(-7.50807322282844,-0.640695822001223,
3.84825558476824));
#12196=CARTESIAN_POINT('Ctrl Pts',(-7.23924588079012,-0.782272634525382,
3.85984901862582));
#12197=CARTESIAN_POINT('Ctrl Pts',(-6.8357314622921,-0.829131775621971,
3.87532291717216));
#12198=CARTESIAN_POINT('Ctrl Pts',(-6.35327616573594,-0.59781018040019,
3.89469527550241));
#12199=CARTESIAN_POINT('Ctrl Pts',(-6.11713987966773,0.00207052637070815,
3.91799017117406));
#12200=CARTESIAN_POINT('Ctrl Pts',(-6.35307678245142,0.602907531120579,
3.94133291042122));
#12201=CARTESIAN_POINT('Ctrl Pts',(-6.93566081689883,0.883875082041324,
3.96472352664209));
#12202=CARTESIAN_POINT('Ctrl Pts',(-7.55515623959697,0.69295296286722,3.98816179669967));
#12203=CARTESIAN_POINT('Ctrl Pts',(-7.88013810709561,0.130810632835588,
4.01164757955687));
#12204=CARTESIAN_POINT('Ctrl Pts',(-7.73550042824472,-0.504166213312069,
4.03518059168276));
#12205=CARTESIAN_POINT('Ctrl Pts',(-7.25691555291904,-0.829965934756777,
4.05614067290557));
#12206=CARTESIAN_POINT('Ctrl Pts',(-6.76789466611817,-0.816273162480241,
4.07451081161441));
#12207=CARTESIAN_POINT('Ctrl Pts',(-6.40500652557533,-0.607330529488023,
4.09027725224445));
#12208=CARTESIAN_POINT('Ctrl Pts',(-6.18597544009142,-0.248853481949266,
4.10606432834162));
#12209=CARTESIAN_POINT('Ctrl Pts',(-6.16476183860982,0.170855301645688,
4.1218718654511));
#12210=CARTESIAN_POINT('Ctrl Pts',(-6.3475351341277,0.550140873965967,4.13769986829671));
#12211=CARTESIAN_POINT('Ctrl Pts',(-6.66120500560645,0.775526485791483,
4.15222680408194));
#12212=CARTESIAN_POINT('Ctrl Pts',(-7.00205431618851,0.839831878170417,
4.16544832658668));
#12213=CARTESIAN_POINT('Ctrl Pts',(-7.30908336124065,0.781894279466921,
4.17735870006853));
#12214=CARTESIAN_POINT('Ctrl Pts',(-7.57377766559882,0.615484497922989,
4.18928029921752));
#12215=CARTESIAN_POINT('Ctrl Pts',(-7.75993041088309,0.363580471659928,
4.20121293126314));
#12216=CARTESIAN_POINT('Ctrl Pts',(-7.84051159534739,0.0612598680482373,
4.21315653403017));
#12217=CARTESIAN_POINT('Ctrl Pts',(-7.79502050738924,-0.3551661585163,4.22909611233079));
#12218=CARTESIAN_POINT('Ctrl Pts',(-7.520840575019,-0.69919923882563,4.24505660563019));
#12219=CARTESIAN_POINT('Ctrl Pts',(-7.12391614845427,-0.836671814188821,
4.26103935959678));
#12220=CARTESIAN_POINT('Ctrl Pts',(-6.80983700920401,-0.825379971791792,
4.27303686635832));
#12221=CARTESIAN_POINT('Ctrl Pts',(-6.5209788758192,-0.699206911902937,
4.28504501164974));
#12222=CARTESIAN_POINT('Ctrl Pts',(-6.29801755032192,-0.4764180427961,4.29706359373192));
#12223=CARTESIAN_POINT('Ctrl Pts',(-6.17188017799352,-0.187148419627673,
4.3090925578342));
#12224=CARTESIAN_POINT('Ctrl Pts',(-6.15992888821969,0.128470193897301,
4.32113188034415));
#12225=CARTESIAN_POINT('Ctrl Pts',(-6.26445823392466,0.426710184996707,
4.33318130259563));
#12226=CARTESIAN_POINT('Ctrl Pts',(-6.5049581998047,0.706766049163178,4.34725107983906));
#12227=CARTESIAN_POINT('Ctrl Pts',(-6.90326744518671,0.872503536145515,
4.36334696251586));
#12228=CARTESIAN_POINT('Ctrl Pts',(-7.38281029184237,0.790877765138433,
4.38147673975636));
#12229=CARTESIAN_POINT('Ctrl Pts',(-7.74572176421123,0.466691558041768,
4.39962862353129));
#12230=CARTESIAN_POINT('Ctrl Pts',(-7.88075906451644,-0.00163370218810728,
4.41780197870862));
#12231=CARTESIAN_POINT('Ctrl Pts',(-7.74575034874242,-0.470472473332599,
4.4359965458689));
#12232=CARTESIAN_POINT('Ctrl Pts',(-7.38159674501435,-0.796028387119033,
4.45421188622969));
#12233=CARTESIAN_POINT('Ctrl Pts',(-6.89950908277415,-0.878014102013699,
4.47244763868539));
#12234=CARTESIAN_POINT('Ctrl Pts',(-6.44720261643851,-0.690747124710534,
4.49070339435891));
#12235=CARTESIAN_POINT('Ctrl Pts',(-6.1635529610742,-0.291109214224599,
4.50897875507623));
#12236=CARTESIAN_POINT('Ctrl Pts',(-6.13597125160479,0.198699563497598,
4.52727330335656));
#12237=CARTESIAN_POINT('Ctrl Pts',(-6.37346031508276,0.628542467914837,
4.54558662808959));
#12238=CARTESIAN_POINT('Ctrl Pts',(-6.80365868518738,0.866395911895694,
4.56391827748347));
#12239=CARTESIAN_POINT('Ctrl Pts',(-7.29496543480093,0.838858349286866,
4.58226786138585));
#12240=CARTESIAN_POINT('Ctrl Pts',(-7.69664252566589,0.553931788000972,
4.60063481598526));
#12241=CARTESIAN_POINT('Ctrl Pts',(-7.88544935552637,0.0984229027900429,
4.61901894616799));
#12242=CARTESIAN_POINT('Ctrl Pts',(-7.81642268275138,-0.306825472701288,
4.63435246271745));
#12243=CARTESIAN_POINT('Ctrl Pts',(-7.6384752345081,-0.572297394360716,
4.64662804193218));
#12244=CARTESIAN_POINT('Ctrl Pts',(-7.39450780779738,-0.778951033732389,
4.6589089055924));
#12245=CARTESIAN_POINT('Ctrl Pts',(-6.99888600622643,-0.893209786912865,
4.67426881313452));
#12246=CARTESIAN_POINT('Ctrl Pts',(-6.52343435780138,-0.756238112350475,
4.69271630273848));
#12247=CARTESIAN_POINT('Ctrl Pts',(-6.19353907010138,-0.38716921999977,
4.71117825554814));
#12248=CARTESIAN_POINT('Ctrl Pts',(-6.11047969071254,0.101292654240927,
4.72965444234953));
#12249=CARTESIAN_POINT('Ctrl Pts',(-6.30018765284877,0.559379591273636,
4.7481442280249));
#12250=CARTESIAN_POINT('Ctrl Pts',(-6.70482157814926,0.846542371924633,
4.76664715301658));
#12251=CARTESIAN_POINT('Ctrl Pts',(-7.20056270996627,0.874413303374147,
4.78516266216818));
#12252=CARTESIAN_POINT('Ctrl Pts',(-7.63543291420515,0.634124121998299,
4.80369025418887));
#12253=CARTESIAN_POINT('Ctrl Pts',(-7.87597488452673,0.198982319936917,
4.8222293469264));
#12254=CARTESIAN_POINT('Ctrl Pts',(-7.84811680670301,-0.297641763084105,
4.8407794771796));
#12255=CARTESIAN_POINT('Ctrl Pts',(-7.5602099822393,-0.703770114540898,
4.85933989842883));
#12256=CARTESIAN_POINT('Ctrl Pts',(-7.10005207809272,-0.894083431664867,
4.87791045675167));
#12257=CARTESIAN_POINT('Ctrl Pts',(-6.60892470845569,-0.810928286707249,
4.89649198113447));
#12258=CARTESIAN_POINT('Ctrl Pts',(-6.23721493477519,-0.478496418619897,
4.91507955704552));
#12259=CARTESIAN_POINT('Ctrl Pts',(-6.14524645745769,-0.1595934132457,4.92748136616133));
#12260=CARTESIAN_POINT('Ctrl Pts',(-6.14522490872935,0.000623928402563829,
4.93367829887062));
#12261=CARTESIAN_POINT('Ctrl Pts',(-6.14410050409056,-0.00048591577833035,
1.06275739095565));
#12262=CARTESIAN_POINT('Ctrl Pts',(-6.14412207724039,0.159913661349453,
1.06896137214896));
#12263=CARTESIAN_POINT('Ctrl Pts',(-6.23622929144067,0.47922381214816,1.08138051738368));
#12264=CARTESIAN_POINT('Ctrl Pts',(-6.60844007459979,0.8121004889077,1.09999411362412));
#12265=CARTESIAN_POINT('Ctrl Pts',(-7.1002710567507,0.895387320978274,1.11860340208149));
#12266=CARTESIAN_POINT('Ctrl Pts',(-7.56113081871182,0.704794039986598,
1.13720366503272));
#12267=CARTESIAN_POINT('Ctrl Pts',(-7.84953105077671,0.29801802119025,1.15579741148642));
#12268=CARTESIAN_POINT('Ctrl Pts',(-7.87744617007159,-0.199444272232843,
1.17438121295457));
#12269=CARTESIAN_POINT('Ctrl Pts',(-7.63650373307356,-0.635363371911168,
1.192955922617));
#12270=CARTESIAN_POINT('Ctrl Pts',(-7.20080576831759,-0.876103765907077,
1.21152037655879));
#12271=CARTESIAN_POINT('Ctrl Pts',(-6.70415725883354,-0.848183653696337,
1.23007445249145));
#12272=CARTESIAN_POINT('Ctrl Pts',(-6.29857446753047,-0.560427267789544,
1.24861722602105));
#12273=CARTESIAN_POINT('Ctrl Pts',(-6.14039323611512,-0.177880372686661,
1.26406029904333));
#12274=CARTESIAN_POINT('Ctrl Pts',(-6.14989802726945,0.143427644563409,
1.2764078954173));
#12275=CARTESIAN_POINT('Ctrl Pts',(-6.2470304684292,0.449740527003316,1.2887513666884));
#12276=CARTESIAN_POINT('Ctrl Pts',(-6.52237137413574,0.75811907727139,1.3041737332961));
#12277=CARTESIAN_POINT('Ctrl Pts',(-6.99898578295027,0.895317551226051,
1.3226669278757));
#12278=CARTESIAN_POINT('Ctrl Pts',(-7.47505081224439,0.758114363165164,
1.34114661424288));
#12279=CARTESIAN_POINT('Ctrl Pts',(-7.80495431777145,0.388892460514594,
1.35961201601459));
#12280=CARTESIAN_POINT('Ctrl Pts',(-7.88775781679195,-0.0988491436399237,
1.37806276650224));
#12281=CARTESIAN_POINT('Ctrl Pts',(-7.69854028573051,-0.555520196691456,
1.39649832149178));
#12282=CARTESIAN_POINT('Ctrl Pts',(-7.29569627612792,-0.841277260574458,
1.41491822157768));
#12283=CARTESIAN_POINT('Ctrl Pts',(-6.80299959078561,-0.86888494277178,
1.43332198328018));
#12284=CARTESIAN_POINT('Ctrl Pts',(-6.37152153031215,-0.630343777158989,
1.4517091401951));
#12285=CARTESIAN_POINT('Ctrl Pts',(-6.13331261235062,-0.199204052893853,
1.47007923391518));
#12286=CARTESIAN_POINT('Ctrl Pts',(-6.16097031239077,0.29211742748464,1.4884318061235));
#12287=CARTESIAN_POINT('Ctrl Pts',(-6.44550960543965,0.693025905897973,
1.50676641948554));
#12288=CARTESIAN_POINT('Ctrl Pts',(-6.89927742024254,0.880903934890723,
1.52508263139204));
#12289=CARTESIAN_POINT('Ctrl Pts',(-7.38295020622619,0.79866296575333,1.54338002563818));
#12290=CARTESIAN_POINT('Ctrl Pts',(-7.74834974407646,0.472007046947655,
1.56165816198871));
#12291=CARTESIAN_POINT('Ctrl Pts',(-7.88379136539645,0.0015932228150884,
1.57991668890152));
#12292=CARTESIAN_POINT('Ctrl Pts',(-7.74836207707285,-0.468425528948212,
1.59815508413406));
#12293=CARTESIAN_POINT('Ctrl Pts',(-7.44470643423547,-0.739409180084324,
1.61333689773705));
#12294=CARTESIAN_POINT('Ctrl Pts',(-7.14358065498685,-0.83487032164026,
1.62547158256094));
#12295=CARTESIAN_POINT('Ctrl Pts',(-6.82794859576551,-0.84421204181463,
1.63759925840241));
#12296=CARTESIAN_POINT('Ctrl Pts',(-6.46957391377044,-0.695762871566993,
1.65207286856862));
#12297=CARTESIAN_POINT('Ctrl Pts',(-6.19976126317667,-0.339120077397132,
1.66888349074963));
#12298=CARTESIAN_POINT('Ctrl Pts',(-6.13589629964516,0.0846784598942406,
1.68500450708744));
#12299=CARTESIAN_POINT('Ctrl Pts',(-6.2824074133963,0.487111860626291,1.70110795274312));
#12300=CARTESIAN_POINT('Ctrl Pts',(-6.60319657410942,0.770074716109897,
1.71719366153553));
#12301=CARTESIAN_POINT('Ctrl Pts',(-7.01969476173132,0.865111288516179,
1.73326137514033));
#12302=CARTESIAN_POINT('Ctrl Pts',(-7.4306928078077,0.749411346956209,1.74931089435423));
#12303=CARTESIAN_POINT('Ctrl Pts',(-7.7354220185315,0.45175405795709,1.76534199326832));
#12304=CARTESIAN_POINT('Ctrl Pts',(-7.87573129698657,-0.000424291859933977,
1.78313350574046));
#12305=CARTESIAN_POINT('Ctrl Pts',(-7.72768926849582,-0.5115400388969,1.8026773859338));
#12306=CARTESIAN_POINT('Ctrl Pts',(-7.25623748727849,-0.850272059219606,
1.82396401709854));
#12307=CARTESIAN_POINT('Ctrl Pts',(-6.72636750519522,-0.82766223357698,
1.84344526759864));
#12308=CARTESIAN_POINT('Ctrl Pts',(-6.34471506576865,-0.552133547071731,
1.86113015122148));
#12309=CARTESIAN_POINT('Ctrl Pts',(-6.16128171743482,-0.171634315548159,
1.87702681595704));
#12310=CARTESIAN_POINT('Ctrl Pts',(-6.18240969119849,0.250208795734504,
1.89290359619399));
#12311=CARTESIAN_POINT('Ctrl Pts',(-6.40235309302082,0.609934372469904,
1.90876032957526));
#12312=CARTESIAN_POINT('Ctrl Pts',(-6.76705946071901,0.820428504223453,
1.92459690112763));
#12313=CARTESIAN_POINT('Ctrl Pts',(-7.18765603844751,0.830971128018649,
1.94041310898236));
#12314=CARTESIAN_POINT('Ctrl Pts',(-7.49890147790259,0.670990327777045,
1.95357632534897));
#12315=CARTESIAN_POINT('Ctrl Pts',(-7.67951671280284,0.465859266917597,
1.96409665265068));
#12316=CARTESIAN_POINT('Ctrl Pts',(-7.8043767947787,0.222944738654196,1.97461011272258));
#12317=CARTESIAN_POINT('Ctrl Pts',(-7.83917648143533,-0.124419817932346,
1.98773878468873));
#12318=CARTESIAN_POINT('Ctrl Pts',(-7.67672672626751,-0.509974597233562,
2.00347273819115));
#12319=CARTESIAN_POINT('Ctrl Pts',(-7.34990055604162,-0.770583214113921,
2.01918541233071));
#12320=CARTESIAN_POINT('Ctrl Pts',(-6.97321369524517,-0.836592625313303,
2.03356972932625));
#12321=CARTESIAN_POINT('Ctrl Pts',(-6.64228894118503,-0.747654759769428,
2.04663120532969));
#12322=CARTESIAN_POINT('Ctrl Pts',(-6.39438122166063,-0.564827652399831,
2.05837453042368));
#12323=CARTESIAN_POINT('Ctrl Pts',(-6.23076075497057,-0.304172929347532,
2.07010604415484));
#12324=CARTESIAN_POINT('Ctrl Pts',(-6.17353255087278,-0.00207671493773103,
2.08182557707505));
#12325=CARTESIAN_POINT('Ctrl Pts',(-6.23075516145379,0.299589335459152,
2.09353321005446));
#12326=CARTESIAN_POINT('Ctrl Pts',(-6.39393436245754,0.55960479989559,2.10522886005712));
#12327=CARTESIAN_POINT('Ctrl Pts',(-6.64058776547682,0.741023493503706,
2.11691253477686));
#12328=CARTESIAN_POINT('Ctrl Pts',(-7.03497389811195,0.848068440992084,
2.13247484644387));
#12329=CARTESIAN_POINT('Ctrl Pts',(-7.54770624434186,0.690428321903564,
2.15189724253272));
#12330=CARTESIAN_POINT('Ctrl Pts',(-7.86933514613633,0.132858902880382,
2.17515629625777));
#12331=CARTESIAN_POINT('Ctrl Pts',(-7.72615768132878,-0.492675738532521,
2.19836709561093));
#12332=CARTESIAN_POINT('Ctrl Pts',(-7.19681213796589,-0.853377790664305,
2.2215297913067));
#12333=CARTESIAN_POINT('Ctrl Pts',(-6.56474624880106,-0.75781946082691,
2.24464435055119));
#12334=CARTESIAN_POINT('Ctrl Pts',(-6.16722750860373,-0.258948675165486,
2.26771088327184));
#12335=CARTESIAN_POINT('Ctrl Pts',(-6.2150427332084,0.37583414834438,2.29072949788041));
#12336=CARTESIAN_POINT('Ctrl Pts',(-6.68088653563404,0.807733315243065,
2.31370036331483));
#12337=CARTESIAN_POINT('Ctrl Pts',(-7.31482602441585,0.807489047368646,
2.3366236806125));
#12338=CARTESIAN_POINT('Ctrl Pts',(-7.77841287257781,0.377009500959829,
2.35949969509982));
#12339=CARTESIAN_POINT('Ctrl Pts',(-7.82534987879143,-0.252577161845689,
2.38232869014123));
#12340=CARTESIAN_POINT('Ctrl Pts',(-7.43233507498677,-0.745015046067986,
2.40511098975844));
#12341=CARTESIAN_POINT('Ctrl Pts',(-6.81055800597004,-0.838490467640577,
2.42784695662596));
#12342=CARTESIAN_POINT('Ctrl Pts',(-6.29223116029819,-0.484813997427444,
2.45053699256128));
#12343=CARTESIAN_POINT('Ctrl Pts',(-6.15310912579615,0.125775995325234,
2.47318153832518));
#12344=CARTESIAN_POINT('Ctrl Pts',(-6.46580906475682,0.666919744066789,
2.4957810706093));
#12345=CARTESIAN_POINT('Ctrl Pts',(-7.06192948798325,0.850560608805366,
2.51833610880894));
#12346=CARTESIAN_POINT('Ctrl Pts',(-7.62273575658636,0.580234313774985,
2.540847196889));
#12347=CARTESIAN_POINT('Ctrl Pts',(-7.84952792540534,0.00176358429277413,
2.5633149405221));
#12348=CARTESIAN_POINT('Ctrl Pts',(-7.62277137533754,-0.575494391866743,
2.58573992305321));
#12349=CARTESIAN_POINT('Ctrl Pts',(-7.0649305920516,-0.84380626649313,2.60812288483676));
#12350=CARTESIAN_POINT('Ctrl Pts',(-6.47468764585225,-0.66166382004421,
2.63046431487488));
#12351=CARTESIAN_POINT('Ctrl Pts',(-6.16628249672348,-0.127049888527898,
2.65276536643547));
#12352=CARTESIAN_POINT('Ctrl Pts',(-6.28109568951485,0.372277207765494,
2.67131565746007));
#12353=CARTESIAN_POINT('Ctrl Pts',(-6.5572455755856,0.646536190026674,2.68613740871844));
#12354=CARTESIAN_POINT('Ctrl Pts',(-6.82386434223888,0.763331776026648,
2.69724384027595));
#12355=CARTESIAN_POINT('Ctrl Pts',(-7.11493971367238,0.774008603859367,
2.70834079855829));
#12356=CARTESIAN_POINT('Ctrl Pts',(-7.38944668657708,0.678048009398333,
2.71942828774665));
#12357=CARTESIAN_POINT('Ctrl Pts',(-7.60966929275022,0.488376278032324,
2.73050641293604));
#12358=CARTESIAN_POINT('Ctrl Pts',(-7.74544261192189,0.231671245772344,
2.74157546675068));
#12359=CARTESIAN_POINT('Ctrl Pts',(-7.77772886818201,-0.0566091099164064,
2.75263518601118));
#12360=CARTESIAN_POINT('Ctrl Pts',(-7.69046381966352,-0.383448777027424,
2.7655283700859));
#12361=CARTESIAN_POINT('Ctrl Pts',(-7.42793832658348,-0.677972215900527,
2.78024752493643));
#12362=CARTESIAN_POINT('Ctrl Pts',(-7.00142534461877,-0.800550675798575,
2.79678644393065));
#12363=CARTESIAN_POINT('Ctrl Pts',(-6.57584982407145,-0.677886291073977,
2.81330669294018));
#12364=CARTESIAN_POINT('Ctrl Pts',(-6.28096997251176,-0.347844732473953,
2.82980813170021));
#12365=CARTESIAN_POINT('Ctrl Pts',(-6.20701576130477,0.087946621438888,
2.84629140165672));
#12366=CARTESIAN_POINT('Ctrl Pts',(-6.37604987195121,0.495869638733109,
2.86275677095718));
#12367=CARTESIAN_POINT('Ctrl Pts',(-6.73581844360051,0.751061859313513,
2.87920481096959));
#12368=CARTESIAN_POINT('Ctrl Pts',(-7.17579711332225,0.775699888633669,
2.89563572893505));
#12369=CARTESIAN_POINT('Ctrl Pts',(-7.56098334322159,0.562728770502053,
2.91205046024346));
#12370=CARTESIAN_POINT('Ctrl Pts',(-7.77381762277454,0.177780339918829,
2.9284483865883));
#12371=CARTESIAN_POINT('Ctrl Pts',(-7.74883414009467,-0.260807751918227,
2.94483239278502));
#12372=CARTESIAN_POINT('Ctrl Pts',(-7.49484470645772,-0.618768936824925,
2.96120009423831));
#12373=CARTESIAN_POINT('Ctrl Pts',(-7.08967346068793,-0.786546626739717,
2.97755335807742));
#12374=CARTESIAN_POINT('Ctrl Pts',(-6.657720721054,-0.713102971741213,2.99389252871196));
#12375=CARTESIAN_POINT('Ctrl Pts',(-6.33131642826648,-0.421337174951404,
3.01021815369535));
#12376=CARTESIAN_POINT('Ctrl Pts',(-6.21026692128662,-0.000967189591566242,
3.02653071397231));
#12377=CARTESIAN_POINT('Ctrl Pts',(-6.33132572760332,0.419054026871033,
3.04283074169105));
#12378=CARTESIAN_POINT('Ctrl Pts',(-6.65705238030844,0.710078042192075,
3.05911874973318));
#12379=CARTESIAN_POINT('Ctrl Pts',(-7.08738278568895,0.783150283438538,
3.07539527341508));
#12380=CARTESIAN_POINT('Ctrl Pts',(-7.49036008893511,0.61618814273907,3.09166084345137));
#12381=CARTESIAN_POINT('Ctrl Pts',(-7.74258151597761,0.260650101302873,
3.10791600264155));
#12382=CARTESIAN_POINT('Ctrl Pts',(-7.76697304166341,-0.174317653031718,
3.12416129945641));
#12383=CARTESIAN_POINT('Ctrl Pts',(-7.5563317668102,-0.555374412970227,
3.14039727791897));
#12384=CARTESIAN_POINT('Ctrl Pts',(-7.17544889508143,-0.765844413327437,
3.15662450083269));
#12385=CARTESIAN_POINT('Ctrl Pts',(-6.74118880081162,-0.74142681352133,
3.17284352210207));
#12386=CARTESIAN_POINT('Ctrl Pts',(-6.38664706125572,-0.489831708198072,
3.18905490924575));
#12387=CARTESIAN_POINT('Ctrl Pts',(-6.22037527072638,-0.0883484616098797,
3.20525922558141));
#12388=CARTESIAN_POINT('Ctrl Pts',(-6.29315956054544,0.339887540079846,
3.22145704360919));
#12389=CARTESIAN_POINT('Ctrl Pts',(-6.58251550195127,0.663644624899192,
3.23764893882998));
#12390=CARTESIAN_POINT('Ctrl Pts',(-6.99963072329188,0.783793247219456,
3.2538354815312));
#12391=CARTESIAN_POINT('Ctrl Pts',(-7.41661272017152,0.663644809896155,
3.27001725696222));
#12392=CARTESIAN_POINT('Ctrl Pts',(-7.70568527679105,0.340149677083231,
3.28619484143681));
#12393=CARTESIAN_POINT('Ctrl Pts',(-7.7783261618395,-0.0874615956887984,
3.30236882102331));
#12394=CARTESIAN_POINT('Ctrl Pts',(-7.61236302022633,-0.488103619326867,
3.31853977629767));
#12395=CARTESIAN_POINT('Ctrl Pts',(-7.25873847420674,-0.739003460387096,
3.33470829571519));
#12396=CARTESIAN_POINT('Ctrl Pts',(-6.82587846889915,-0.763306477612443,
3.35087496493719));
#12397=CARTESIAN_POINT('Ctrl Pts',(-6.44646523023161,-0.55360846219804,
3.36704036914161));
#12398=CARTESIAN_POINT('Ctrl Pts',(-6.23677704618538,-0.174209133649937,
3.38320509172753));
#12399=CARTESIAN_POINT('Ctrl Pts',(-6.26108481548361,0.258592599799861,
3.39936973132143));
#12400=CARTESIAN_POINT('Ctrl Pts',(-6.51192371113038,0.612138413508131,
3.41553483603588));
#12401=CARTESIAN_POINT('Ctrl Pts',(-6.91246725256316,0.778040033227508,
3.43170106480072));
#12402=CARTESIAN_POINT('Ctrl Pts',(-7.33986110031951,0.705423732658014,
3.44786881262982));
#12403=CARTESIAN_POINT('Ctrl Pts',(-7.66330225180869,0.416455198735406,
3.46403905603656));
#12404=CARTESIAN_POINT('Ctrl Pts',(-7.76314448110752,0.0691836941953803,
3.47751601213562));
#12405=CARTESIAN_POINT('Ctrl Pts',(-7.72348592779732,-0.208769115260678,
3.48830037788075));
#12406=CARTESIAN_POINT('Ctrl Pts',(-7.60915687709694,-0.465286651701113,
3.49908593215301));
#12407=CARTESIAN_POINT('Ctrl Pts',(-7.33982769226549,-0.706235104211514,
3.51256903136456));
#12408=CARTESIAN_POINT('Ctrl Pts',(-6.91163155362933,-0.779188237324528,
3.52875357310865));
#12409=CARTESIAN_POINT('Ctrl Pts',(-6.55548444266184,-0.63109352619522,
3.54314470826614));
#12410=CARTESIAN_POINT('Ctrl Pts',(-6.34011871400958,-0.38036708219665,
3.55574171383355));
#12411=CARTESIAN_POINT('Ctrl Pts',(-6.24639647450997,-0.113075731347263,
3.56654128345746));
#12412=CARTESIAN_POINT('Ctrl Pts',(-6.2571004711447,0.170138823557678,3.57734399581171));
#12413=CARTESIAN_POINT('Ctrl Pts',(-6.37034993489611,0.429980603706305,
3.58814957433025));
#12414=CARTESIAN_POINT('Ctrl Pts',(-6.57092700052057,0.630418764957175,
3.59895848058192));
#12415=CARTESIAN_POINT('Ctrl Pts',(-6.830850714758,0.743936015163079,3.60977063520182));
#12416=CARTESIAN_POINT('Ctrl Pts',(-7.11441971427059,0.754517996689564,
3.62058700132255));
#12417=CARTESIAN_POINT('Ctrl Pts',(-7.32278052411025,0.68159756714758,3.62900216988483));
#12418=CARTESIAN_POINT('Ctrl Pts',(-7.50391457198171,0.561381429877749,
3.6374197054472));
#12419=CARTESIAN_POINT('Ctrl Pts',(-7.67348487864857,0.374325256349744,
3.64704230565885));
#12420=CARTESIAN_POINT('Ctrl Pts',(-7.77729848202131,0.0380717430195915,
3.66027880858025));
#12421=CARTESIAN_POINT('Ctrl Pts',(-7.69804120365716,-0.354373328164954,
3.67532745719795));
#12422=CARTESIAN_POINT('Ctrl Pts',(-7.41848398951318,-0.667534119421154,
3.69098736267498));
#12423=CARTESIAN_POINT('Ctrl Pts',(-6.9990632960658,-0.788379913874128,
3.70726054669447));
#12424=CARTESIAN_POINT('Ctrl Pts',(-6.57948025538097,-0.667512143973283,
3.72354511539254));
#12425=CARTESIAN_POINT('Ctrl Pts',(-6.28822210540625,-0.341703386586052,
3.73984162248617));
#12426=CARTESIAN_POINT('Ctrl Pts',(-6.214947252681,0.0895247616185924,3.75615047657178));
#12427=CARTESIAN_POINT('Ctrl Pts',(-6.38236889523311,0.493801790031738,
3.77247232162259));
#12428=CARTESIAN_POINT('Ctrl Pts',(-6.73967995056519,0.747643053294839,
3.78880728997579));
#12429=CARTESIAN_POINT('Ctrl Pts',(-7.12863355815078,0.768970568205483,
3.80334000325068));
#12430=CARTESIAN_POINT('Ctrl Pts',(-7.43455531549802,0.635168646195069,
3.81606611806074));
#12431=CARTESIAN_POINT('Ctrl Pts',(-7.6371093846873,0.432883606871512,3.8269804250519));
#12432=CARTESIAN_POINT('Ctrl Pts',(-7.75160187649833,0.170239682165284,
3.8379015715229));
#12433=CARTESIAN_POINT('Ctrl Pts',(-7.76244105669299,-0.116247652674151,
3.84882949139145));
#12434=CARTESIAN_POINT('Ctrl Pts',(-7.66763793861865,-0.386911128974891,
3.85976441318346));
#12435=CARTESIAN_POINT('Ctrl Pts',(-7.48047767628426,-0.604726336185073,
3.87070649501486));
#12436=CARTESIAN_POINT('Ctrl Pts',(-7.22657273961852,-0.738431388646221,
3.88165581413315));
#12437=CARTESIAN_POINT('Ctrl Pts',(-6.84559484715752,-0.782659505496549,
3.89626492121388));
#12438=CARTESIAN_POINT('Ctrl Pts',(-6.39035895969544,-0.564314377486963,
3.91454454394013));
#12439=CARTESIAN_POINT('Ctrl Pts',(-6.16773943366211,0.00142552218543602,
3.93651217130362));
#12440=CARTESIAN_POINT('Ctrl Pts',(-6.39017049813292,0.567679522925422,
3.95851150179096));
#12441=CARTESIAN_POINT('Ctrl Pts',(-6.93898016017053,0.83229149877013,3.98054457232659));
#12442=CARTESIAN_POINT('Ctrl Pts',(-7.52223705917294,0.652480441661669,
4.0026118930303));
#12443=CARTESIAN_POINT('Ctrl Pts',(-7.82804385744497,0.123409451029175,
4.02471464764302));
#12444=CARTESIAN_POINT('Ctrl Pts',(-7.69193113695034,-0.473949690379908,
4.04685362373763));
#12445=CARTESIAN_POINT('Ctrl Pts',(-7.24181863438223,-0.780329262527218,
4.06656588170735));
#12446=CARTESIAN_POINT('Ctrl Pts',(-6.7820134805878,-0.767442446346911,
4.08383853386223));
#12447=CARTESIAN_POINT('Ctrl Pts',(-6.44086041985743,-0.571004816225905,
4.09866082654509));
#12448=CARTESIAN_POINT('Ctrl Pts',(-6.2349792076924,-0.234034685896682,
4.11350056349035));
#12449=CARTESIAN_POINT('Ctrl Pts',(-6.21504713433741,0.160446370067885,
4.12835806169351));
#12450=CARTESIAN_POINT('Ctrl Pts',(-6.3868236701026,0.51690216155789,4.14323345115286));
#12451=CARTESIAN_POINT('Ctrl Pts',(-6.68160097485276,0.728706442019366,
4.15688557825564));
#12452=CARTESIAN_POINT('Ctrl Pts',(-7.0019056807236,0.789135115020865,4.16931021399055));
#12453=CARTESIAN_POINT('Ctrl Pts',(-7.29042452641039,0.734688640425214,
4.18050272820112));
#12454=CARTESIAN_POINT('Ctrl Pts',(-7.53916074485403,0.578311269612235,
4.19170571187556));
#12455=CARTESIAN_POINT('Ctrl Pts',(-7.71409171667038,0.341590655634556,
4.20291927766093));
#12456=CARTESIAN_POINT('Ctrl Pts',(-7.7898177049696,0.0574856270825079,
4.21414344977244));
#12457=CARTESIAN_POINT('Ctrl Pts',(-7.74706612373166,-0.333862955380633,
4.22912337531477));
#12458=CARTESIAN_POINT('Ctrl Pts',(-7.48937849541761,-0.657211178204218,
4.24412476954085));
#12459=CARTESIAN_POINT('Ctrl Pts',(-7.11628554615372,-0.786433878154665,
4.25914816467973));
#12460=CARTESIAN_POINT('Ctrl Pts',(-6.82103578880878,-0.77581930313266,
4.2704267350549));
#12461=CARTESIAN_POINT('Ctrl Pts',(-6.5494657022935,-0.657201742063754,
4.28171637563045));
#12462=CARTESIAN_POINT('Ctrl Pts',(-6.33982460180875,-0.447724590754319,
4.29301720482683));
#12463=CARTESIAN_POINT('Ctrl Pts',(-6.2212038304369,-0.175704823349057,
4.30432922595009));
#12464=CARTESIAN_POINT('Ctrl Pts',(-6.20996096390589,0.12113566135513,4.31565255452681));
#12465=CARTESIAN_POINT('Ctrl Pts',(-6.3082813903755,0.401676910179385,4.32698721417064));
#12466=CARTESIAN_POINT('Ctrl Pts',(-6.53453931041383,0.665155379172314,
4.34022426133603));
#12467=CARTESIAN_POINT('Ctrl Pts',(-6.90934792817869,0.821130796703102,
4.3553714888365));
#12468=CARTESIAN_POINT('Ctrl Pts',(-7.36074527364388,0.744316254597853,
4.37243815749654));
#12469=CARTESIAN_POINT('Ctrl Pts',(-7.7024754750817,0.43907929924283,4.38953088858621));
#12470=CARTESIAN_POINT('Ctrl Pts',(-7.82969309329709,-0.00204137070426244,
4.40664990380937));
#12471=CARTESIAN_POINT('Ctrl Pts',(-7.70250067292396,-0.443824957085235,
4.42379531432277));
#12472=CARTESIAN_POINT('Ctrl Pts',(-7.3592455074783,-0.750732264321921,
4.44096726291832));
#12473=CARTESIAN_POINT('Ctrl Pts',(-6.90461076111005,-0.828077026739987,
4.45816585671055));
#12474=CARTESIAN_POINT('Ctrl Pts',(-6.47785145640082,-0.651418695241634,
4.47539120143168));
#12475=CARTESIAN_POINT('Ctrl Pts',(-6.21007591581231,-0.274199129165646,
4.49264338319947));
#12476=CARTESIAN_POINT('Ctrl Pts',(-6.18399470172574,0.188387346819458,
4.50992248166671));
#12477=CARTESIAN_POINT('Ctrl Pts',(-6.40837539543801,0.594574778942697,
4.52722855314471));
#12478=CARTESIAN_POINT('Ctrl Pts',(-6.81509167143493,0.819485331368328,
4.54456166410994));
#12479=CARTESIAN_POINT('Ctrl Pts',(-7.27987319414489,0.793471678330472,
4.56192181882538));
#12480=CARTESIAN_POINT('Ctrl Pts',(-7.66011479470359,0.523796174615442,
4.57930912132998));
#12481=CARTESIAN_POINT('Ctrl Pts',(-7.83898719320449,0.0923657793623214,
4.59672341312303));
#12482=CARTESIAN_POINT('Ctrl Pts',(-7.77359845357327,-0.29173800569068,
4.61125815306387));
#12483=CARTESIAN_POINT('Ctrl Pts',(-7.60486413396222,-0.543478230712311,
4.62289900894297));
#12484=CARTESIAN_POINT('Ctrl Pts',(-7.37344723337822,-0.739509772796316,
4.63454888242984));
#12485=CARTESIAN_POINT('Ctrl Pts',(-6.99796916640192,-0.847988290174798,
4.64912877493909));
#12486=CARTESIAN_POINT('Ctrl Pts',(-6.54638127238998,-0.717940114779771,
4.6666513290107));
#12487=CARTESIAN_POINT('Ctrl Pts',(-6.232781786496,-0.367178113186201,4.68420096407712));
#12488=CARTESIAN_POINT('Ctrl Pts',(-6.15372371672015,0.0974436948677159,
4.70177742940139));
#12489=CARTESIAN_POINT('Ctrl Pts',(-6.33426751835694,0.533542705055676,
4.71938074720947));
#12490=CARTESIAN_POINT('Ctrl Pts',(-6.7197391499259,0.807173042125499,4.73701077817937));
#12491=CARTESIAN_POINT('Ctrl Pts',(-7.19242759577209,0.833802363418686,
4.75466748667689));
#12492=CARTESIAN_POINT('Ctrl Pts',(-7.60745560394516,0.60453864229177,4.77235067103721));
#12493=CARTESIAN_POINT('Ctrl Pts',(-7.83725063197469,0.188941390247915,
4.79006042872509));
#12494=CARTESIAN_POINT('Ctrl Pts',(-7.8106711862218,-0.285829700854973,
4.80779618745207));
#12495=CARTESIAN_POINT('Ctrl Pts',(-7.53521563022957,-0.674475138957433,
4.82555885140828));
#12496=CARTESIAN_POINT('Ctrl Pts',(-7.09452497559831,-0.856799563884475,
4.84334606079258));
#12497=CARTESIAN_POINT('Ctrl Pts',(-6.62369779984497,-0.777148624143293,
4.86115986092763));
#12498=CARTESIAN_POINT('Ctrl Pts',(-6.26696887582568,-0.458201653067476,
4.87899721597154));
#12499=CARTESIAN_POINT('Ctrl Pts',(-6.17856731994658,-0.151930989278767,
4.89090963520109));
#12500=CARTESIAN_POINT('Ctrl Pts',(-6.17854660968293,0.00205226831345774,
4.89686544420304));
#12501=CARTESIAN_POINT('Ctrl Pts',(-6.15532181468697,0.00138488703415226,
1.01435007802725));
#12502=CARTESIAN_POINT('Ctrl Pts',(-6.1553431152372,0.159757645663868,1.02047566534903));
#12503=CARTESIAN_POINT('Ctrl Pts',(-6.24623111421967,0.475075705756006,
1.03273758175489));
#12504=CARTESIAN_POINT('Ctrl Pts',(-6.61422672853683,0.80433161688607,1.05114350930259));
#12505=CARTESIAN_POINT('Ctrl Pts',(-7.10116639540294,0.886859556533852,
1.06956675049812));
#12506=CARTESIAN_POINT('Ctrl Pts',(-7.55806039306351,0.698002185192178,
1.08800459577221));
#12507=CARTESIAN_POINT('Ctrl Pts',(-7.8443721167838,0.294291635454448,1.1064570708697));
#12508=CARTESIAN_POINT('Ctrl Pts',(-7.87219577959167,-0.200096078911815,
1.12492425022168));
#12509=CARTESIAN_POINT('Ctrl Pts',(-7.63250722014404,-0.633915270826186,
1.14340533646129));
#12510=CARTESIAN_POINT('Ctrl Pts',(-7.19844236190399,-0.87385140291206,
1.16189996598086));
#12511=CARTESIAN_POINT('Ctrl Pts',(-6.70297864922338,-0.846086645447464,
1.1804074750247));
#12512=CARTESIAN_POINT('Ctrl Pts',(-6.2978047958826,-0.558728259760231,
1.19892754958468));
#12513=CARTESIAN_POINT('Ctrl Pts',(-6.139538539105,-0.176162993711043,1.2143705962764));
#12514=CARTESIAN_POINT('Ctrl Pts',(-6.14903967530696,0.145501856680318,
1.22673123417169));
#12515=CARTESIAN_POINT('Ctrl Pts',(-6.24632555571259,0.452346696169204,
1.239095571006));
#12516=CARTESIAN_POINT('Ctrl Pts',(-6.52234008288225,0.761589519917251,
1.25455717363935));
#12517=CARTESIAN_POINT('Ctrl Pts',(-7.00080290977026,0.899413229449575,
1.27312169979619));
#12518=CARTESIAN_POINT('Ctrl Pts',(-7.47936561468606,0.761578690439182,
1.29169587691259));
#12519=CARTESIAN_POINT('Ctrl Pts',(-7.81146685686393,0.390026773641098,
1.31027931928451));
#12520=CARTESIAN_POINT('Ctrl Pts',(-7.89499560809641,-0.101473505781537,
1.3288713963235));
#12521=CARTESIAN_POINT('Ctrl Pts',(-7.70415448553098,-0.562288126274461,
1.34747158083016));
#12522=CARTESIAN_POINT('Ctrl Pts',(-7.29722514506761,-0.851048902454855,
1.3660792909068));
#12523=CARTESIAN_POINT('Ctrl Pts',(-6.79885441200529,-0.879060781972192,
1.38469396999124));
#12524=CARTESIAN_POINT('Ctrl Pts',(-6.36181870759125,-0.63754524480614,
1.40331504129361));
#12525=CARTESIAN_POINT('Ctrl Pts',(-6.12019073027554,-0.200394147677602,
1.42194193808049));
#12526=CARTESIAN_POINT('Ctrl Pts',(-6.14818632446221,0.298444301700259,
1.4405740774677));
#12527=CARTESIAN_POINT('Ctrl Pts',(-6.43736173956987,0.706031374616256,
1.45921088701331));
#12528=CARTESIAN_POINT('Ctrl Pts',(-6.89916431053514,0.897327322215646,
1.4778517860215));
#12529=CARTESIAN_POINT('Ctrl Pts',(-7.39204751091533,0.813605469747302,
1.49649618519644));
#12530=CARTESIAN_POINT('Ctrl Pts',(-7.76489965161589,0.480398984552206,
1.51514351443042));
#12531=CARTESIAN_POINT('Ctrl Pts',(-7.90332809212511,-8.96281492521594E-5,
1.53379315987099));
#12532=CARTESIAN_POINT('Ctrl Pts',(-7.7649060157838,-0.480792699234354,
1.55244459112492));
#12533=CARTESIAN_POINT('Ctrl Pts',(-7.45403998538145,-0.75829949879398,
1.56798834125249));
#12534=CARTESIAN_POINT('Ctrl Pts',(-7.14544718809111,-0.856141214202644,
1.58042376628376));
#12535=CARTESIAN_POINT('Ctrl Pts',(-6.82180196362564,-0.865733441257941,
1.592859283437));
#12536=CARTESIAN_POINT('Ctrl Pts',(-6.45398629112311,-0.713440752735991,
1.60771267399531));
#12537=CARTESIAN_POINT('Ctrl Pts',(-6.17673186358275,-0.347059455508924,
1.62498362624803));
#12538=CARTESIAN_POINT('Ctrl Pts',(-6.11099778616178,0.0887865953086014,
1.64156282477639));
#12539=CARTESIAN_POINT('Ctrl Pts',(-6.26177741085195,0.503103111464865,
1.6581407399915));
#12540=CARTESIAN_POINT('Ctrl Pts',(-6.5923194610229,0.794739465687361,1.67471694279706));
#12541=CARTESIAN_POINT('Ctrl Pts',(-7.02193769700808,0.892823305180966,
1.69129102758754));
#12542=CARTESIAN_POINT('Ctrl Pts',(-7.44632452845763,0.773409502201043,
1.70786259019089));
#12543=CARTESIAN_POINT('Ctrl Pts',(-7.76130934158841,0.46580285735598,1.72443120336651));
#12544=CARTESIAN_POINT('Ctrl Pts',(-7.90651951677609,-0.00196807962334312,
1.74283704477602));
#12545=CARTESIAN_POINT('Ctrl Pts',(-7.75330353635983,-0.531346850232141,
1.76307810860955));
#12546=CARTESIAN_POINT('Ctrl Pts',(-7.26449796556357,-0.882702447669824,
1.78515164667195));
#12547=CARTESIAN_POINT('Ctrl Pts',(-6.71436229145052,-0.859335279308994,
1.80537779316638));
#12548=CARTESIAN_POINT('Ctrl Pts',(-6.3176646664297,-0.573013323811329,
1.82375837638183));
#12549=CARTESIAN_POINT('Ctrl Pts',(-6.12680833020744,-0.177218873527421,
1.84029511474842));
#12550=CARTESIAN_POINT('Ctrl Pts',(-6.14875890700447,0.261990487464417,
1.85682569031829));
#12551=CARTESIAN_POINT('Ctrl Pts',(-6.37791553494525,0.636870862801446,
1.87334973144588));
#12552=CARTESIAN_POINT('Ctrl Pts',(-6.7582629833497,0.856443868873814,1.8898667925222));
#12553=CARTESIAN_POINT('Ctrl Pts',(-7.19729006439147,0.867492922871737,
1.90637662966974));
#12554=CARTESIAN_POINT('Ctrl Pts',(-7.52245896265695,0.700396003581133,
1.92012822956414));
#12555=CARTESIAN_POINT('Ctrl Pts',(-7.71126282344545,0.485974231171035,
1.93112537636886));
#12556=CARTESIAN_POINT('Ctrl Pts',(-7.84183705801084,0.231956797192165,
1.94211976155069));
#12557=CARTESIAN_POINT('Ctrl Pts',(-7.87828239403315,-0.131509317473049,
1.95585786032622));
#12558=CARTESIAN_POINT('Ctrl Pts',(-7.70820816241811,-0.535261941489649,
1.97233415651205));
#12559=CARTESIAN_POINT('Ctrl Pts',(-7.36572329095194,-0.80840715001223,
1.98880189639337));
#12560=CARTESIAN_POINT('Ctrl Pts',(-6.97067541231049,-0.877668187533008,
2.00388811678008));
#12561=CARTESIAN_POINT('Ctrl Pts',(-6.62339026681109,-0.78435311697415,
2.01759537265686));
#12562=CARTESIAN_POINT('Ctrl Pts',(-6.3630812755978,-0.592396239794856,
2.02992631914616));
#12563=CARTESIAN_POINT('Ctrl Pts',(-6.19117506852127,-0.318573480034593,
2.04225125653785));
#12564=CARTESIAN_POINT('Ctrl Pts',(-6.13101025620552,-0.0010421798929461,
2.05457019344336));
#12565=CARTESIAN_POINT('Ctrl Pts',(-6.19117175900474,0.316205694335182,
2.06688287651045));
#12566=CARTESIAN_POINT('Ctrl Pts',(-6.36285264509343,0.589792470866144,
2.07918920353492));
#12567=CARTESIAN_POINT('Ctrl Pts',(-6.62249464601974,0.780782662724837,
2.09148902616807));
#12568=CARTESIAN_POINT('Ctrl Pts',(-7.0378498001605,0.89353864001136,2.10787980243138));
#12569=CARTESIAN_POINT('Ctrl Pts',(-7.57827502836269,0.727484904857922,
2.12835184441199));
#12570=CARTESIAN_POINT('Ctrl Pts',(-7.91766293688888,0.139356339769869,
2.15288956866496));
#12571=CARTESIAN_POINT('Ctrl Pts',(-7.76659689250598,-0.521123950569987,
2.17739794495675));
#12572=CARTESIAN_POINT('Ctrl Pts',(-7.20729504630159,-0.902360411029734,
2.20187569995981));
#12573=CARTESIAN_POINT('Ctrl Pts',(-6.53885375332028,-0.801399036365866,
2.2263218674333));
#12574=CARTESIAN_POINT('Ctrl Pts',(-6.11808523348063,-0.273493855561213,
2.25073537703529));
#12575=CARTESIAN_POINT('Ctrl Pts',(-6.16864061548512,0.398778645678198,
2.27511524207653));
#12576=CARTESIAN_POINT('Ctrl Pts',(-6.66226090036659,0.856536394347886,
2.29946047535543));
#12577=CARTESIAN_POINT('Ctrl Pts',(-7.33447899690987,0.856349278793802,
2.32377013175939));
#12578=CARTESIAN_POINT('Ctrl Pts',(-7.82637817814363,0.399669335099744,
2.34804328860591));
#12579=CARTESIAN_POINT('Ctrl Pts',(-7.8762624403739,-0.268644644505232,
2.3722790575478));
#12580=CARTESIAN_POINT('Ctrl Pts',(-7.45891773050366,-0.791653462716088,
2.39647657914323));
#12581=CARTESIAN_POINT('Ctrl Pts',(-6.79831471817344,-0.891013892478177,
2.42063502780583));
#12582=CARTESIAN_POINT('Ctrl Pts',(-6.24739027927042,-0.515144657685069,
2.44475360957481));
#12583=CARTESIAN_POINT('Ctrl Pts',(-6.09944401021374,0.134016413694163,
2.46883156460017));
#12584=CARTESIAN_POINT('Ctrl Pts',(-6.43196540399374,0.709519549341717,
2.49286816857682));
#12585=CARTESIAN_POINT('Ctrl Pts',(-7.06605101482765,0.904879456246692,
2.51686272802793));
#12586=CARTESIAN_POINT('Ctrl Pts',(-7.6626855728488,0.617300900309224,2.54081459614203));
#12587=CARTESIAN_POINT('Ctrl Pts',(-7.90400060789426,0.00181430507667405,
2.56472313989482));
#12588=CARTESIAN_POINT('Ctrl Pts',(-7.66272120125994,-0.612424319707219,
2.58858781519659));
#12589=CARTESIAN_POINT('Ctrl Pts',(-7.06913692438929,-0.897923665578739,
2.61240800689291));
#12590=CARTESIAN_POINT('Ctrl Pts',(-6.44110784712269,-0.704106841661814,
2.63618339293661));
#12591=CARTESIAN_POINT('Ctrl Pts',(-6.11300163800619,-0.13530675007174,
2.6599131277551));
#12592=CARTESIAN_POINT('Ctrl Pts',(-6.23516444880693,0.395865212665747,
2.67965031459637));
#12593=CARTESIAN_POINT('Ctrl Pts',(-6.52887561201059,0.687563852182344,
2.69541600209137));
#12594=CARTESIAN_POINT('Ctrl Pts',(-6.81242451351045,0.811765155919268,
2.70722885200896));
#12595=CARTESIAN_POINT('Ctrl Pts',(-7.12193899701994,0.823119375286228,
2.71902998121532));
#12596=CARTESIAN_POINT('Ctrl Pts',(-7.41379212450475,0.721083917159786,
2.73081943099457));
#12597=CARTESIAN_POINT('Ctrl Pts',(-7.64789851807236,0.519457544257522,
2.74259717622193));
#12598=CARTESIAN_POINT('Ctrl Pts',(-7.79219812426804,0.246613467879735,
2.75436301193177));
#12599=CARTESIAN_POINT('Ctrl Pts',(-7.82650908620457,-0.0597313562161861,
2.7661172444166));
#12600=CARTESIAN_POINT('Ctrl Pts',(-7.73378757716163,-0.406973488614899,
2.77981611351335));
#12601=CARTESIAN_POINT('Ctrl Pts',(-7.45492482469592,-0.71980366041697,
2.7954531697841));
#12602=CARTESIAN_POINT('Ctrl Pts',(-7.00202657290324,-0.849945537810255,
2.81301855620783));
#12603=CARTESIAN_POINT('Ctrl Pts',(-6.55031472914827,-0.719724882478119,
2.83055666346136));
#12604=CARTESIAN_POINT('Ctrl Pts',(-6.23746400207544,-0.36953503313781,
2.84806791497705));
#12605=CARTESIAN_POINT('Ctrl Pts',(-6.15906083953478,0.0926443368691964,
2.86555208259416));
#12606=CARTESIAN_POINT('Ctrl Pts',(-6.33827503896183,0.525051519501817,
2.88300927653526));
#12607=CARTESIAN_POINT('Ctrl Pts',(-6.71948296038623,0.795408929008851,
2.9004393700713));
#12608=CARTESIAN_POINT('Ctrl Pts',(-7.18541682404627,0.821461485746422,
2.91784256578514));
#12609=CARTESIAN_POINT('Ctrl Pts',(-7.59308397004501,0.596020867715862,
2.93521846564008));
#12610=CARTESIAN_POINT('Ctrl Pts',(-7.81818529244133,0.188794732061472,
2.95256800644698));
#12611=CARTESIAN_POINT('Ctrl Pts',(-7.7917393257621,-0.274841348485349,
2.96988919463305));
#12612=CARTESIAN_POINT('Ctrl Pts',(-7.52336307186317,-0.652997969583897,
2.98718447937879));
#12613=CARTESIAN_POINT('Ctrl Pts',(-7.09557333299563,-0.830093838469998,
3.00445276553991));
#12614=CARTESIAN_POINT('Ctrl Pts',(-6.63984770037723,-0.752562258100537,
3.02169424976486));
#12615=CARTESIAN_POINT('Ctrl Pts',(-6.29575429265797,-0.444921405411109,
3.03890898207291));
#12616=CARTESIAN_POINT('Ctrl Pts',(-6.16827535941431,-0.0020478494357645,
3.05609707435848));
#12617=CARTESIAN_POINT('Ctrl Pts',(-6.29576084516153,0.440087461163198,
3.07325862942099));
#12618=CARTESIAN_POINT('Ctrl Pts',(-6.63840792454696,0.746158494232759,
3.09039376920604));
#12619=CARTESIAN_POINT('Ctrl Pts',(-7.09068019304077,0.822901273377244,
3.10750262488744));
#12620=CARTESIAN_POINT('Ctrl Pts',(-7.51381249206245,0.647527693807565,
3.12458534015527));
#12621=CARTESIAN_POINT('Ctrl Pts',(-7.77838184349055,0.274483967111054,
3.1416420706223));
#12622=CARTESIAN_POINT('Ctrl Pts',(-7.80388976455076,-0.181448994759944,
3.15867298547141));
#12623=CARTESIAN_POINT('Ctrl Pts',(-7.5832500525651,-0.580467956848055,
3.17567826210021));
#12624=CARTESIAN_POINT('Ctrl Pts',(-7.18473556223459,-0.800610040459843,
3.19265809517254));
#12625=CARTESIAN_POINT('Ctrl Pts',(-6.73085657140814,-0.775025767238161,
3.20961268663487));
#12626=CARTESIAN_POINT('Ctrl Pts',(-6.36070451906988,-0.512273567169555,
3.22654225372828));
#12627=CARTESIAN_POINT('Ctrl Pts',(-6.18733396966188,-0.0934765731086235,
3.24344702281474));
#12628=CARTESIAN_POINT('Ctrl Pts',(-6.26323916414107,0.352718866884148,
3.26032723384026));
#12629=CARTESIAN_POINT('Ctrl Pts',(-6.5644653146297,0.689654189913989,3.27718313896965));
#12630=CARTESIAN_POINT('Ctrl Pts',(-6.99816156269536,0.814506053793651,
3.29401499779763));
#12631=CARTESIAN_POINT('Ctrl Pts',(-7.43119591985385,0.689658200052887,
3.31082308735104));
#12632=CARTESIAN_POINT('Ctrl Pts',(-7.73101487965898,0.354028369562565,
3.32760769072432));
#12633=CARTESIAN_POINT('Ctrl Pts',(-7.80621008929764,-0.0890580187097431,
3.34436910576017));
#12634=CARTESIAN_POINT('Ctrl Pts',(-7.63437921518094,-0.503670252109045,
3.3611076385834));
#12635=CARTESIAN_POINT('Ctrl Pts',(-7.26879300011845,-0.762964363645185,
3.37782360837663));
#12636=CARTESIAN_POINT('Ctrl Pts',(-6.82188403144782,-0.787979502772466,
3.39451734656986));
#12637=CARTESIAN_POINT('Ctrl Pts',(-6.43068068140195,-0.571676584050765,
3.41118918856227));
#12638=CARTESIAN_POINT('Ctrl Pts',(-6.21479487163316,-0.180901065491681,
3.42783949414826));
#12639=CARTESIAN_POINT('Ctrl Pts',(-6.23987688745805,0.264266034793347,
3.44446861244254));
#12640=CARTESIAN_POINT('Ctrl Pts',(-6.49762030296562,0.627403516828641,
3.46107694553375));
#12641=CARTESIAN_POINT('Ctrl Pts',(-6.90858155892206,0.79753201259649,3.47766481821013));
#12642=CARTESIAN_POINT('Ctrl Pts',(-7.34647065959468,0.723048174829234,
3.49423276489497));
#12643=CARTESIAN_POINT('Ctrl Pts',(-7.67737022510294,0.427306551784298,
3.51078089929711));
#12644=CARTESIAN_POINT('Ctrl Pts',(-7.77933122717147,0.0724197403299812,
3.52455543522332));
#12645=CARTESIAN_POINT('Ctrl Pts',(-7.73883473089208,-0.211307153844965,
3.53556486182041));
#12646=CARTESIAN_POINT('Ctrl Pts',(-7.62219195347972,-0.472977173161771,
3.54656812666788));
#12647=CARTESIAN_POINT('Ctrl Pts',(-7.34766442127358,-0.718477552599507,
3.56031169704533));
#12648=CARTESIAN_POINT('Ctrl Pts',(-6.91186389572488,-0.792629818951791,
3.57678586132189));
#12649=CARTESIAN_POINT('Ctrl Pts',(-6.54994772408427,-0.642052793745427,
3.59141379637521));
#12650=CARTESIAN_POINT('Ctrl Pts',(-6.33135654406045,-0.387527817989315,
3.60420144661415));
#12651=CARTESIAN_POINT('Ctrl Pts',(-6.23633570855798,-0.116439386124594,
3.61515526155727));
#12652=CARTESIAN_POINT('Ctrl Pts',(-6.24720382915164,0.170515824271984,
3.62610159770129));
#12653=CARTESIAN_POINT('Ctrl Pts',(-6.36187322079165,0.433535026443583,
3.63704090051234));
#12654=CARTESIAN_POINT('Ctrl Pts',(-6.56473431971144,0.636227626371285,
3.64797311424009));
#12655=CARTESIAN_POINT('Ctrl Pts',(-6.82736797498893,0.750897209952491,
3.658898542734));
#12656=CARTESIAN_POINT('Ctrl Pts',(-7.11359555037847,0.761558159597187,
3.66981678486612));
#12657=CARTESIAN_POINT('Ctrl Pts',(-7.32371319540262,0.688003016744239,
3.67830393871623));
#12658=CARTESIAN_POINT('Ctrl Pts',(-7.50625823729936,0.566851651520274,
3.68678751070037));
#12659=CARTESIAN_POINT('Ctrl Pts',(-7.67702206646534,0.378444857690304,
3.69647907721837));
#12660=CARTESIAN_POINT('Ctrl Pts',(-7.78141257136081,0.0401475505155527,
3.70979636942345));
#12661=CARTESIAN_POINT('Ctrl Pts',(-7.70171508493293,-0.354162708398042,
3.72491902485287));
#12662=CARTESIAN_POINT('Ctrl Pts',(-7.42114612466325,-0.668341455127249,
3.74063460686844));
#12663=CARTESIAN_POINT('Ctrl Pts',(-7.00088080163629,-0.789344259007442,
3.75694185015021));
#12664=CARTESIAN_POINT('Ctrl Pts',(-6.58110712328952,-0.668334279667831,
3.77323691251503));
#12665=CARTESIAN_POINT('Ctrl Pts',(-6.29018412194349,-0.34277049623807,
3.78952031471304));
#12666=CARTESIAN_POINT('Ctrl Pts',(-6.21717139609482,0.0874524632090739,
3.80579265961626));
#12667=CARTESIAN_POINT('Ctrl Pts',(-6.38403928177642,0.490161525526526,
3.82205440992407));
#12668=CARTESIAN_POINT('Ctrl Pts',(-6.73954376788978,0.742605706624229,
3.83830635307579));
#12669=CARTESIAN_POINT('Ctrl Pts',(-7.1259124951814,0.763713676639482,3.85274389917685));
#12670=CARTESIAN_POINT('Ctrl Pts',(-7.42942016411094,0.630936102189617,
3.86537059518623));
#12671=CARTESIAN_POINT('Ctrl Pts',(-7.6301784569546,0.430405395217166,3.87618990189906));
#12672=CARTESIAN_POINT('Ctrl Pts',(-7.74353726685436,0.170304121516873,
3.88700551322282));
#12673=CARTESIAN_POINT('Ctrl Pts',(-7.75423281912403,-0.113134514061421,
3.89781770500068));
#12674=CARTESIAN_POINT('Ctrl Pts',(-7.66050792598422,-0.380656665238867,
3.90862661199449));
#12675=CARTESIAN_POINT('Ctrl Pts',(-7.47566669878727,-0.595729520002875,
3.91943237649964));
#12676=CARTESIAN_POINT('Ctrl Pts',(-7.22516692240344,-0.727621081205731,
3.93023521909756));
#12677=CARTESIAN_POINT('Ctrl Pts',(-6.84964587248811,-0.771177648449039,
3.94463520824916));
#12678=CARTESIAN_POINT('Ctrl Pts',(-6.40163159698102,-0.556119063029255,
3.96262903315017));
#12679=CARTESIAN_POINT('Ctrl Pts',(-6.18311346213355,-0.000224236590168895,
3.98421206227288));
#12680=CARTESIAN_POINT('Ctrl Pts',(-6.40142810194215,0.555005154061987,
4.00578771530793));
#12681=CARTESIAN_POINT('Ctrl Pts',(-6.93874203129211,0.813853076380022,
4.02735679834234));
#12682=CARTESIAN_POINT('Ctrl Pts',(-7.50861106416408,0.637962848998229,
4.04892096810037));
#12683=CARTESIAN_POINT('Ctrl Pts',(-7.80673620650473,0.121794509865376,
4.07048149068405));
#12684=CARTESIAN_POINT('Ctrl Pts',(-7.67400892248061,-0.459829671966149,
4.0920398259536));
#12685=CARTESIAN_POINT('Ctrl Pts',(-7.23638059365412,-0.75751561964237,
4.11120202311155));
#12686=CARTESIAN_POINT('Ctrl Pts',(-6.79005425730626,-0.744940744569275,
4.1279693946883));
#12687=CARTESIAN_POINT('Ctrl Pts',(-6.45928263693368,-0.554426517452247,
4.14234208150331));
#12688=CARTESIAN_POINT('Ctrl Pts',(-6.25991541608282,-0.228019663351229,
4.15671586125759));
#12689=CARTESIAN_POINT('Ctrl Pts',(-6.24068116030339,0.15365327946892,4.1710910801691));
#12690=CARTESIAN_POINT('Ctrl Pts',(-6.40674558298073,0.498142296774453,
4.1854682482322));
#12691=CARTESIAN_POINT('Ctrl Pts',(-6.69137279180131,0.702599429114232,
4.19864939667764));
#12692=CARTESIAN_POINT('Ctrl Pts',(-7.00034153191099,0.760867123384676,
4.21063430004806));
#12693=CARTESIAN_POINT('Ctrl Pts',(-7.27843068823313,0.70836902278032,4.22142238458483));
#12694=CARTESIAN_POINT('Ctrl Pts',(-7.5179857131659,0.557741775949331,4.23221238061628));
#12695=CARTESIAN_POINT('Ctrl Pts',(-7.68632465558915,0.329907804903081,
4.24300440013838));
#12696=CARTESIAN_POINT('Ctrl Pts',(-7.75913469605848,0.0566828026146494,
4.25379865262834));
#12697=CARTESIAN_POINT('Ctrl Pts',(-7.7180202023265,-0.319402775086334,
4.26819421301669));
#12698=CARTESIAN_POINT('Ctrl Pts',(-7.47057957124159,-0.629743130547593,
4.28259470202932));
#12699=CARTESIAN_POINT('Ctrl Pts',(-7.11280162175997,-0.753630952420848,
4.29700123189475));
#12700=CARTESIAN_POINT('Ctrl Pts',(-6.82986918527034,-0.743445233993496,
4.30780913559938));
#12701=CARTESIAN_POINT('Ctrl Pts',(-6.56981457045782,-0.629837115749421,
4.31862032283963));
#12702=CARTESIAN_POINT('Ctrl Pts',(-6.36920262800273,-0.429359709312094,
4.32943489251995));
#12703=CARTESIAN_POINT('Ctrl Pts',(-6.25577547078144,-0.169206543388766,
4.34025305726424));
#12704=CARTESIAN_POINT('Ctrl Pts',(-6.24504644209274,0.114494238429322,
4.35107497032088));
#12705=CARTESIAN_POINT('Ctrl Pts',(-6.33896947900305,0.38243886083468,4.36190076276199));
#12706=CARTESIAN_POINT('Ctrl Pts',(-6.55495387030909,0.633924630661768,
4.37453573308082));
#12707=CARTESIAN_POINT('Ctrl Pts',(-6.9124614167636,0.782648524492007,4.38898251478319));
#12708=CARTESIAN_POINT('Ctrl Pts',(-7.34259808028965,0.709396411557978,
4.40524507600026));
#12709=CARTESIAN_POINT('Ctrl Pts',(-7.66792322353676,0.418743989320809,
4.42151836634654));
#12710=CARTESIAN_POINT('Ctrl Pts',(-7.78889500630819,-0.000902978993542901,
4.43780279177667));
#12711=CARTESIAN_POINT('Ctrl Pts',(-7.66795110493541,-0.420807930740282,
4.45409892771709));
#12712=CARTESIAN_POINT('Ctrl Pts',(-7.34191240663444,-0.712259181511612,
4.47040727724938));
#12713=CARTESIAN_POINT('Ctrl Pts',(-6.91044557617938,-0.785616858356274,
4.4867283632995));
#12714=CARTESIAN_POINT('Ctrl Pts',(-6.50575685387359,-0.618047933668166,
4.50306269522463));
#12715=CARTESIAN_POINT('Ctrl Pts',(-6.25203399164393,-0.260552904403482,
4.51941078451858));
#12716=CARTESIAN_POINT('Ctrl Pts',(-6.22737477948063,0.17751833719177,4.53577312557919));
#12717=CARTESIAN_POINT('Ctrl Pts',(-6.43975685988429,0.561906946644777,
4.5521502223111));
#12718=CARTESIAN_POINT('Ctrl Pts',(-6.82444025681707,0.774592630399746,
4.56854254120903));
#12719=CARTESIAN_POINT('Ctrl Pts',(-7.26375799435716,0.74996988957729,4.58495060473737));
#12720=CARTESIAN_POINT('Ctrl Pts',(-7.62294571861381,0.495187693439224,
4.60137479256222));
#12721=CARTESIAN_POINT('Ctrl Pts',(-7.79180148886195,0.0878321179432545,
4.6178157625393));
#12722=CARTESIAN_POINT('Ctrl Pts',(-7.73007153353779,-0.274632525096982,
4.63153055763558));
#12723=CARTESIAN_POINT('Ctrl Pts',(-7.57089063696386,-0.512111859070372,
4.64251171031102));
#12724=CARTESIAN_POINT('Ctrl Pts',(-7.35262771058493,-0.696995379209438,
4.65349879703564));
#12725=CARTESIAN_POINT('Ctrl Pts',(-6.99862347533104,-0.799249420049326,
4.66724321525578));
#12726=CARTESIAN_POINT('Ctrl Pts',(-6.5730502033671,-0.676668689478975,
4.68375532144801));
#12727=CARTESIAN_POINT('Ctrl Pts',(-6.27764603292305,-0.346222659526638,
4.70028617112997));
#12728=CARTESIAN_POINT('Ctrl Pts',(-6.20321862496408,0.0913138303420951,
4.71683637846958));
#12729=CARTESIAN_POINT('Ctrl Pts',(-6.3731989872548,0.501843406155816,4.73340624603523));
#12730=CARTESIAN_POINT('Ctrl Pts',(-6.7359781539714,0.75934304394148,4.74999621871112));
#12731=CARTESIAN_POINT('Ctrl Pts',(-7.18070827957232,0.78438157978822,4.7666066278755));
#12732=CARTESIAN_POINT('Ctrl Pts',(-7.5710873754965,0.568720907705442,4.78323791268823));
#12733=CARTESIAN_POINT('Ctrl Pts',(-7.7871878954453,0.177879522683858,4.79989027648649));
#12734=CARTESIAN_POINT('Ctrl Pts',(-7.76219315364765,-0.268520028593769,
4.81656438241647));
#12735=CARTESIAN_POINT('Ctrl Pts',(-7.50325083995188,-0.633887980333893,
4.83325981631157));
#12736=CARTESIAN_POINT('Ctrl Pts',(-7.08900958601159,-0.805258128798486,
4.84997847660876));
#12737=CARTESIAN_POINT('Ctrl Pts',(-6.64648651499231,-0.730418221478834,
4.86671963489532));
#12738=CARTESIAN_POINT('Ctrl Pts',(-6.31122984273527,-0.430620194746299,
4.88348417172117));
#12739=CARTESIAN_POINT('Ctrl Pts',(-6.22817497301499,-0.14287585295958,
4.89467473489709));
#12740=CARTESIAN_POINT('Ctrl Pts',(-6.22815549748057,0.00192704684477944,
4.9002754633636));
#12741=CARTESIAN_POINT('Ctrl Pts',(-6.18504029502821,0.00193448151638033,
1.00003735833913));
#12742=CARTESIAN_POINT('Ctrl Pts',(-6.18506085287023,0.154785094133507,
1.00594935850175));
#12743=CARTESIAN_POINT('Ctrl Pts',(-6.27276333944073,0.459023202656318,
1.01778085296466));
#12744=CARTESIAN_POINT('Ctrl Pts',(-6.62802047127092,0.776941905279901,
1.03555190416764));
#12745=CARTESIAN_POINT('Ctrl Pts',(-7.09833345900095,0.856671496747452,
1.05334612192011));
#12746=CARTESIAN_POINT('Ctrl Pts',(-7.53984756346967,0.674214010051848,
1.07116357476926));
#12747=CARTESIAN_POINT('Ctrl Pts',(-7.81668484764973,0.283933690087942,
1.08900405680934));
#12748=CARTESIAN_POINT('Ctrl Pts',(-7.84363617288521,-0.194258242749199,
1.10686720694953));
#12749=CARTESIAN_POINT('Ctrl Pts',(-7.6117174721288,-0.614100052993139,
1.12475288155903));
#12750=CARTESIAN_POINT('Ctrl Pts',(-7.19145858739647,-0.846449404226388,
1.14266083536209));
#12751=CARTESIAN_POINT('Ctrl Pts',(-6.71147351063424,-0.819590956705147,
1.16059082409754));
#12752=CARTESIAN_POINT('Ctrl Pts',(-6.31872073476413,-0.541091061200067,
1.17854264946671));
#12753=CARTESIAN_POINT('Ctrl Pts',(-6.16519721681528,-0.170078173925239,
1.19352038967065));
#12754=CARTESIAN_POINT('Ctrl Pts',(-6.1744086284735,0.142017095597367,1.20551337044202));
#12755=CARTESIAN_POINT('Ctrl Pts',(-6.26882012143519,0.439818968973141,
1.21751340794948));
#12756=CARTESIAN_POINT('Ctrl Pts',(-6.53679306581284,0.740104540264321,
1.2325263267041));
#12757=CARTESIAN_POINT('Ctrl Pts',(-7.00162674500001,0.874047532223047,
1.25056268894745));
#12758=CARTESIAN_POINT('Ctrl Pts',(-7.46686569583001,0.740096839109722,
1.26861943195502));
#12759=CARTESIAN_POINT('Ctrl Pts',(-7.78994676609457,0.378704727073858,
1.28669632216987));
#12760=CARTESIAN_POINT('Ctrl Pts',(-7.87129533220736,-0.0996909691720917,
1.30479301011282));
#12761=CARTESIAN_POINT('Ctrl Pts',(-7.68546305982998,-0.548533502869181,
1.32290918478904));
#12762=CARTESIAN_POINT('Ctrl Pts',(-7.2888893757855,-0.830004177694432,
1.34104450291075));
#12763=CARTESIAN_POINT('Ctrl Pts',(-6.80284662879364,-0.857371495441115,
1.35919862600619));
#12764=CARTESIAN_POINT('Ctrl Pts',(-6.37630721910642,-0.62171240423037,
1.37737119834619));
#12765=CARTESIAN_POINT('Ctrl Pts',(-6.14029008944201,-0.194815129798296,
1.39556186131529));
#12766=CARTESIAN_POINT('Ctrl Pts',(-6.1675992442859,0.292692098595048,1.41377024261863));
#12767=CARTESIAN_POINT('Ctrl Pts',(-6.4503620565862,0.691329238623259,1.43199596178485));
#12768=CARTESIAN_POINT('Ctrl Pts',(-6.90229353244458,0.878592492416463,
1.45023864246069));
#12769=CARTESIAN_POINT('Ctrl Pts',(-7.3850203982638,0.796649505790598,1.46849785770109));
#12770=CARTESIAN_POINT('Ctrl Pts',(-7.75048564762091,0.470116177201949,
1.48677326782443));
#12771=CARTESIAN_POINT('Ctrl Pts',(-7.88631090938092,-0.00114003308241335,
1.50506431154639));
#12772=CARTESIAN_POINT('Ctrl Pts',(-7.75049450355181,-0.472989727708301,
1.52337088433291));
#12773=CARTESIAN_POINT('Ctrl Pts',(-7.44516447734219,-0.745614857762243,
1.53863831810871));
#12774=CARTESIAN_POINT('Ctrl Pts',(-7.14185932067798,-0.841789876750141,
1.55086037195908));
#12775=CARTESIAN_POINT('Ctrl Pts',(-6.82363866744145,-0.851230986545527,
1.5630872130319));
#12776=CARTESIAN_POINT('Ctrl Pts',(-6.4617685488527,-0.701448731340242,
1.57769859306773));
#12777=CARTESIAN_POINT('Ctrl Pts',(-6.18876956484561,-0.34076204481659,
1.59470138391594));
#12778=CARTESIAN_POINT('Ctrl Pts',(-6.12396946764894,0.0886308712451369,
1.6110341660673));
#12779=CARTESIAN_POINT('Ctrl Pts',(-6.27258422281589,0.497118933516093,
1.62737718838713));
#12780=CARTESIAN_POINT('Ctrl Pts',(-6.59866814413671,0.784876696180629,
1.64372989468327));
#12781=CARTESIAN_POINT('Ctrl Pts',(-7.02281705661602,0.881754356975332,
1.66009208771515));
#12782=CARTESIAN_POINT('Ctrl Pts',(-7.44212133414031,0.763816074620149,
1.67646326617426));
#12783=CARTESIAN_POINT('Ctrl Pts',(-7.7535740269982,0.459712179182955,1.69284330156785));
#12784=CARTESIAN_POINT('Ctrl Pts',(-7.89729582298658,-0.00309554884323294,
1.71105347450618));
#12785=CARTESIAN_POINT('Ctrl Pts',(-7.74565582599341,-0.527339088652752,
1.73109590677901));
#12786=CARTESIAN_POINT('Ctrl Pts',(-7.26120105934481,-0.875694925054935,
1.75297406892667));
#12787=CARTESIAN_POINT('Ctrl Pts',(-6.71534965504902,-0.852596704401631,
1.77304116487539));
#12788=CARTESIAN_POINT('Ctrl Pts',(-6.32138409450613,-0.56830758518348,
1.79129152330856));
#12789=CARTESIAN_POINT('Ctrl Pts',(-6.13168016009827,-0.174995072057024,
1.80772340676423));
#12790=CARTESIAN_POINT('Ctrl Pts',(-6.15346807946314,0.261805298226859,
1.8241613205225));
#12791=CARTESIAN_POINT('Ctrl Pts',(-6.3814999287675,0.634928357941657,1.84060479295286));
#12792=CARTESIAN_POINT('Ctrl Pts',(-6.76030269950564,0.853656791887009,
1.85705375788615));
#12793=CARTESIAN_POINT('Ctrl Pts',(-7.19789052510478,0.864714230059756,
1.87350701678844));
#12794=CARTESIAN_POINT('Ctrl Pts',(-7.52226056848553,0.698064177431438,
1.88722279945193));
#12795=CARTESIAN_POINT('Ctrl Pts',(-7.71070782550361,0.484061348889512,
1.89819798603134));
#12796=CARTESIAN_POINT('Ctrl Pts',(-7.84108555720893,0.230444159542277,
1.90917447353455));
#12797=CARTESIAN_POINT('Ctrl Pts',(-7.87753262696172,-0.132633185091885,
1.92289532864967));
#12798=CARTESIAN_POINT('Ctrl Pts',(-7.70754420346973,-0.536305861250017,
1.93936662503784));
#12799=CARTESIAN_POINT('Ctrl Pts',(-7.36494164093582,-0.809602048425494,
1.95583772289023));
#12800=CARTESIAN_POINT('Ctrl Pts',(-6.96941379361634,-0.878990673585998,
1.97094063523801));
#12801=CARTESIAN_POINT('Ctrl Pts',(-6.6214605738567,-0.785512528627816,
1.98467314307479));
#12802=CARTESIAN_POINT('Ctrl Pts',(-6.36049958258628,-0.593104694820152,
1.99703284926989));
#12803=CARTESIAN_POINT('Ctrl Pts',(-6.18806293476214,-0.31846173055547,
2.009393865417));
#12804=CARTESIAN_POINT('Ctrl Pts',(-6.12765851408817,0.000201419297515972,
2.02175553044862));
#12805=CARTESIAN_POINT('Ctrl Pts',(-6.18805878567595,0.318766070561102,
2.03411794133265));
#12806=CARTESIAN_POINT('Ctrl Pts',(-6.36052742775184,0.593653877290259,
2.0464809140462));
#12807=CARTESIAN_POINT('Ctrl Pts',(-6.62153479810473,0.785659877107895,
2.05884415784856));
#12808=CARTESIAN_POINT('Ctrl Pts',(-7.03930435057696,0.899103574502222,
2.07532922744145));
#12809=CARTESIAN_POINT('Ctrl Pts',(-7.58335701362722,0.732049936951038,
2.09593354806076));
#12810=CARTESIAN_POINT('Ctrl Pts',(-7.92551787329716,0.139411230229194,
2.1206590672799));
#12811=CARTESIAN_POINT('Ctrl Pts',(-7.77324093952945,-0.526992586217095,
2.14538184010843));
#12812=CARTESIAN_POINT('Ctrl Pts',(-7.2084092233759,-0.912170787733487,
2.17010128170181));
#12813=CARTESIAN_POINT('Ctrl Pts',(-6.53249969066519,-0.810226392153337,
2.19481578239594));
#12814=CARTESIAN_POINT('Ctrl Pts',(-6.1064692514412,-0.275947007217316,
2.21952419869039));
#12815=CARTESIAN_POINT('Ctrl Pts',(-6.15755851138988,0.405302051662446,
2.24422520707067));
#12816=CARTESIAN_POINT('Ctrl Pts',(-6.65820462432343,0.869765062388611,
2.26891757489148));
#12817=CARTESIAN_POINT('Ctrl Pts',(-7.3408453138212,0.869712680842248,2.29360004643675));
#12818=CARTESIAN_POINT('Ctrl Pts',(-7.84099046916954,0.405562883710353,
2.31827138853594));
#12819=CARTESIAN_POINT('Ctrl Pts',(-7.89188859340855,-0.274527300040944,
2.3429303738485));
#12820=CARTESIAN_POINT('Ctrl Pts',(-7.46684950513523,-0.80739148940899,
2.36757578662995));
#12821=CARTESIAN_POINT('Ctrl Pts',(-6.7932369408934,-0.90884115826819,2.39220642377932));
#12822=CARTESIAN_POINT('Ctrl Pts',(-6.23080912069766,-0.525280033465689,
2.41682109261757));
#12823=CARTESIAN_POINT('Ctrl Pts',(-6.07951966246936,0.137978359245954,
2.44141861634764));
#12824=CARTESIAN_POINT('Ctrl Pts',(-6.41950013676486,0.726640754772934,
2.46599782859082));
#12825=CARTESIAN_POINT('Ctrl Pts',(-7.06860259417947,0.926755491531088,
2.49055758358057));
#12826=CARTESIAN_POINT('Ctrl Pts',(-7.68002986417738,0.632179798873464,
2.5150967369546));
#12827=CARTESIAN_POINT('Ctrl Pts',(-7.92764552134961,0.000944522328351112,
2.53961419282274));
#12828=CARTESIAN_POINT('Ctrl Pts',(-7.68005721336133,-0.629669549355358,
2.56410878618908));
#12829=CARTESIAN_POINT('Ctrl Pts',(-7.07019550228192,-0.923123702908933,
2.5885795656002));
#12830=CARTESIAN_POINT('Ctrl Pts',(-6.42429617364977,-0.723912036667828,
2.61302511363373));
#12831=CARTESIAN_POINT('Ctrl Pts',(-6.08649119115101,-0.138517440976113,
2.63744512150446));
#12832=CARTESIAN_POINT('Ctrl Pts',(-6.21223966684041,0.408665861755775,
2.65777140910349));
#12833=CARTESIAN_POINT('Ctrl Pts',(-6.51498330382994,0.709351113648519,
2.674020274529));
#12834=CARTESIAN_POINT('Ctrl Pts',(-6.80735978088213,0.837439867343505,
2.68619945257517));
#12835=CARTESIAN_POINT('Ctrl Pts',(-7.12664566011944,0.849157334778109,
2.6983714927253));
#12836=CARTESIAN_POINT('Ctrl Pts',(-7.42783351180677,0.743878457965117,
2.71053617994053));
#12837=CARTESIAN_POINT('Ctrl Pts',(-7.66951637957178,0.53572864979586,2.72269330897038));
#12838=CARTESIAN_POINT('Ctrl Pts',(-7.81855579145374,0.253955441206058,
2.73484314375331));
#12839=CARTESIAN_POINT('Ctrl Pts',(-7.85400455176983,-0.062539492106813,
2.74698487897661));
#12840=CARTESIAN_POINT('Ctrl Pts',(-7.75818762301745,-0.421432107598265,
2.76114224858493));
#12841=CARTESIAN_POINT('Ctrl Pts',(-7.46987365614386,-0.744902407746362,
2.77730708509788));
#12842=CARTESIAN_POINT('Ctrl Pts',(-7.00137013388183,-0.879557403138088,
2.79547350221892));
#12843=CARTESIAN_POINT('Ctrl Pts',(-6.53382613240907,-0.744802175259395,
2.81362214087364));
#12844=CARTESIAN_POINT('Ctrl Pts',(-6.20983574866432,-0.382182712148995,
2.83175179566087));
#12845=CARTESIAN_POINT('Ctrl Pts',(-6.12857703292412,0.0966500403142058,
2.84986244064629));
#12846=CARTESIAN_POINT('Ctrl Pts',(-6.31430871100684,0.544862222497401,
2.86795349734992));
#12847=CARTESIAN_POINT('Ctrl Pts',(-6.70959717985322,0.825242975432329,
2.88602481111419));
#12848=CARTESIAN_POINT('Ctrl Pts',(-7.19296888464305,0.852302747612439,
2.90407573088816));
#12849=CARTESIAN_POINT('Ctrl Pts',(-7.6160819344623,0.618348268313813,2.92210658574007));
#12850=CARTESIAN_POINT('Ctrl Pts',(-7.84982079765454,0.195559912762412,
2.94011563526226));
#12851=CARTESIAN_POINT('Ctrl Pts',(-7.82237000115257,-0.286026340065306,
2.95810576365756));
#12852=CARTESIAN_POINT('Ctrl Pts',(-7.54353880028185,-0.678962954634159,
2.97607295385774));
#12853=CARTESIAN_POINT('Ctrl Pts',(-7.09889613896107,-0.863059411748946,
2.99401870845086));
#12854=CARTESIAN_POINT('Ctrl Pts',(-6.62504791383588,-0.782464854277864,
3.01194258453785));
#12855=CARTESIAN_POINT('Ctrl Pts',(-6.26714694908666,-0.462504395091709,
3.02984438133514));
#12856=CARTESIAN_POINT('Ctrl Pts',(-6.13450086477898,-0.0017428437012401,
3.04772383986694));
#12857=CARTESIAN_POINT('Ctrl Pts',(-6.26715807301811,0.458389157575083,
3.06558074068058));
#12858=CARTESIAN_POINT('Ctrl Pts',(-6.62383159683867,0.777010504229039,
3.08341486755061));
#12859=CARTESIAN_POINT('Ctrl Pts',(-7.09474387207995,0.856931067075294,
3.10122601821375));
#12860=CARTESIAN_POINT('Ctrl Pts',(-7.53542180806767,0.674300001519429,
3.11901400258171));
#12861=CARTESIAN_POINT('Ctrl Pts',(-7.81102536987665,0.285718970191242,
3.1367786406439));
#12862=CARTESIAN_POINT('Ctrl Pts',(-7.83761192611158,-0.189300816311006,
3.15451976374402));
#12863=CARTESIAN_POINT('Ctrl Pts',(-7.60770460153743,-0.605099341888002,
3.1722372169101));
#12864=CARTESIAN_POINT('Ctrl Pts',(-7.192377909984,-0.834537764149841,3.18993085280259));
#12865=CARTESIAN_POINT('Ctrl Pts',(-6.71928442386195,-0.807877081114413,
3.20760053887308));
#12866=CARTESIAN_POINT('Ctrl Pts',(-6.33341662752147,-0.533975589038894,
3.22524615138231));
#12867=CARTESIAN_POINT('Ctrl Pts',(-6.1526663682926,-0.0973624004398561,
3.24286758015074));
#12868=CARTESIAN_POINT('Ctrl Pts',(-6.23180408134589,0.367850412115243,
3.26046472470488));
#12869=CARTESIAN_POINT('Ctrl Pts',(-6.5458840541067,0.7191652253215,3.27803749683208));
#12870=CARTESIAN_POINT('Ctrl Pts',(-6.99810294271046,0.849349265206921,
3.29558582036997));
#12871=CARTESIAN_POINT('Ctrl Pts',(-7.44963689661624,0.719166284808225,
3.31310962945538));
#12872=CARTESIAN_POINT('Ctrl Pts',(-7.76226017562776,0.369198513354485,
3.33060887092856));
#12873=CARTESIAN_POINT('Ctrl Pts',(-7.84066094364821,-0.0928017396707875,
3.34808350242358));
#12874=CARTESIAN_POINT('Ctrl Pts',(-7.66149885418233,-0.525088884595006,
3.3655334936625));
#12875=CARTESIAN_POINT('Ctrl Pts',(-7.28034773305643,-0.79541391783641,
3.38295882562499));
#12876=CARTESIAN_POINT('Ctrl Pts',(-6.81445718631064,-0.821483139569074,
3.40035949040031));
#12877=CARTESIAN_POINT('Ctrl Pts',(-6.40668765829451,-0.59600943840361,
3.41773549312221));
#12878=CARTESIAN_POINT('Ctrl Pts',(-6.18169584214414,-0.188728419605418,
3.43508684584969));
#12879=CARTESIAN_POINT('Ctrl Pts',(-6.20784514290506,0.275165281873529,
3.45241358192968));
#12880=CARTESIAN_POINT('Ctrl Pts',(-6.47639639507144,0.653507341417247,
3.46971572219518));
#12881=CARTESIAN_POINT('Ctrl Pts',(-6.90449682661278,0.830715021230648,
3.48699334992386));
#12882=CARTESIAN_POINT('Ctrl Pts',(-7.36054265068983,0.75312759896658,3.50424644156099));
#12883=CARTESIAN_POINT('Ctrl Pts',(-7.70507323679672,0.445177926714059,
3.52147524374292));
#12884=CARTESIAN_POINT('Ctrl Pts',(-7.81119433678745,0.075752404018898,
3.53581204983664));
#12885=CARTESIAN_POINT('Ctrl Pts',(-7.76904314299935,-0.219543515671938,
3.54726986688073));
#12886=CARTESIAN_POINT('Ctrl Pts',(-7.64765861917188,-0.491844914406571,
3.55871960593793));
#12887=CARTESIAN_POINT('Ctrl Pts',(-7.36203942815138,-0.747244560961086,
3.57301619085879));
#12888=CARTESIAN_POINT('Ctrl Pts',(-6.90878559141423,-0.824346342944035,
3.59014821043938));
#12889=CARTESIAN_POINT('Ctrl Pts',(-6.5325070262611,-0.667772572877197,
3.60535557378859));
#12890=CARTESIAN_POINT('Ctrl Pts',(-6.30530616111317,-0.403207986958227,
3.61864694286058));
#12891=CARTESIAN_POINT('Ctrl Pts',(-6.20656869022908,-0.121503914492411,
3.63002891106073));
#12892=CARTESIAN_POINT('Ctrl Pts',(-6.21786904271036,0.17661120472348,3.64140045843225));
#12893=CARTESIAN_POINT('Ctrl Pts',(-6.33697049241504,0.449785070539879,
3.65276160378139));
#12894=CARTESIAN_POINT('Ctrl Pts',(-6.54761646387189,0.660239824218537,
3.66411237271902));
#12895=CARTESIAN_POINT('Ctrl Pts',(-6.82024360477912,0.779264913606105,
3.67545286820712));
#12896=CARTESIAN_POINT('Ctrl Pts',(-7.11728136597602,0.790317129746521,
3.68678318085792));
#12897=CARTESIAN_POINT('Ctrl Pts',(-7.33526250184263,0.714001102786347,
3.69558769336262));
#12898=CARTESIAN_POINT('Ctrl Pts',(-7.52460478021158,0.588335445521869,
3.7043869786929));
#12899=CARTESIAN_POINT('Ctrl Pts',(-7.70168747930115,0.392944569857713,
3.71443734764326));
#12900=CARTESIAN_POINT('Ctrl Pts',(-7.80988273301986,0.0422429930341788,
3.72824225157302));
#12901=CARTESIAN_POINT('Ctrl Pts',(-7.72727513305559,-0.366328708453495,
3.74391125197574));
#12902=CARTESIAN_POINT('Ctrl Pts',(-7.43666554118108,-0.691696849479157,
3.76018685693119));
#12903=CARTESIAN_POINT('Ctrl Pts',(-7.00161691448238,-0.816915579528899,
3.77706653049292));
#12904=CARTESIAN_POINT('Ctrl Pts',(-6.56733396055601,-0.691682810651421,
3.79392454460657));
#12905=CARTESIAN_POINT('Ctrl Pts',(-6.26654562765578,-0.3550205123833,3.81076115841936));
#12906=CARTESIAN_POINT('Ctrl Pts',(-6.1911325553665,0.0895827193733467,
3.82757667281065));
#12907=CARTESIAN_POINT('Ctrl Pts',(-6.36350946096962,0.50548282085585,3.84437132520021));
#12908=CARTESIAN_POINT('Ctrl Pts',(-6.73047124123842,0.766010242524385,
3.86114554454008));
#12909=CARTESIAN_POINT('Ctrl Pts',(-7.12901368034643,0.787746171743655,
3.87603784194693));
#12910=CARTESIAN_POINT('Ctrl Pts',(-7.44190892966169,0.650845344649784,
3.88905532446545));
#12911=CARTESIAN_POINT('Ctrl Pts',(-7.64878134275722,0.444189022830509,
3.90020462760315));
#12912=CARTESIAN_POINT('Ctrl Pts',(-7.76553306778079,0.176269133820623,
3.91134511925484));
#12913=CARTESIAN_POINT('Ctrl Pts',(-7.77653094523285,-0.115552363536951,
3.92247714568019));
#12914=CARTESIAN_POINT('Ctrl Pts',(-7.68006611264172,-0.390854840429437,
3.9336006136539));
#12915=CARTESIAN_POINT('Ctrl Pts',(-7.48992306377386,-0.612073383815134,
3.94471576165104));
#12916=CARTESIAN_POINT('Ctrl Pts',(-7.23237165848447,-0.747663663403516,
3.95582259199976));
#12917=CARTESIAN_POINT('Ctrl Pts',(-6.84646473121294,-0.792403433674334,
3.97062077929395));
#12918=CARTESIAN_POINT('Ctrl Pts',(-6.3864410792178,-0.571475980182002,
3.98909889576364));
#12919=CARTESIAN_POINT('Ctrl Pts',(-6.16238496201624,-0.00115785824039473,
4.01124054191812));
#12920=CARTESIAN_POINT('Ctrl Pts',(-6.3862304211917,0.567803406777749,4.03335240929006));
#12921=CARTESIAN_POINT('Ctrl Pts',(-6.93635510725266,0.832684234789182,
4.05543432814072));
#12922=CARTESIAN_POINT('Ctrl Pts',(-7.51909126085599,0.652689650771393,
4.07748779641409));
#12923=CARTESIAN_POINT('Ctrl Pts',(-7.82352412968288,0.125343566686662,
4.09951350361257));
#12924=CARTESIAN_POINT('Ctrl Pts',(-7.68796000136869,-0.468110630686831,
4.12151270501089));
#12925=CARTESIAN_POINT('Ctrl Pts',(-7.2418525938744,-0.771426362219948,
4.14104449245175));
#12926=CARTESIAN_POINT('Ctrl Pts',(-6.7873808143172,-0.758570879140142,
4.15811957803281));
#12927=CARTESIAN_POINT('Ctrl Pts',(-6.45084731947709,-0.564693301253677,
4.1727448719699));
#12928=CARTESIAN_POINT('Ctrl Pts',(-6.24818669107861,-0.232820084937952,
4.18735958652774));
#12929=CARTESIAN_POINT('Ctrl Pts',(-6.22869241803636,0.154912462764796,
4.20196415138622));
#12930=CARTESIAN_POINT('Ctrl Pts',(-6.39729009617743,0.504573285610341,
4.21655860239769));
#12931=CARTESIAN_POINT('Ctrl Pts',(-6.68600830745319,0.7119144340067,4.22993002217742));
#12932=CARTESIAN_POINT('Ctrl Pts',(-6.99915603726572,0.770953989010427,
4.24207743095502));
#12933=CARTESIAN_POINT('Ctrl Pts',(-7.28083374176742,0.717756806009324,
4.25300578778819));
#12934=CARTESIAN_POINT('Ctrl Pts',(-7.52332570145096,0.565265639900522,
4.26392915087842));
#12935=CARTESIAN_POINT('Ctrl Pts',(-7.69361125094384,0.334758364883805,
4.27484799782803));
#12936=CARTESIAN_POINT('Ctrl Pts',(-7.76721204522818,0.0585123291627315,
4.28576249660097));
#12937=CARTESIAN_POINT('Ctrl Pts',(-7.72563755456501,-0.321492167904461,
4.30030880645676));
#12938=CARTESIAN_POINT('Ctrl Pts',(-7.47577070976408,-0.634729906167413,
4.31484910788061));
#12939=CARTESIAN_POINT('Ctrl Pts',(-7.11494082441407,-0.75964778831911,
4.32937923018361));
#12940=CARTESIAN_POINT('Ctrl Pts',(-6.82977343242683,-0.749363011330386,
4.3402736097982));
#12941=CARTESIAN_POINT('Ctrl Pts',(-6.5678367429364,-0.63491734918943,4.35116416567639));
#12942=CARTESIAN_POINT('Ctrl Pts',(-6.36591104875818,-0.433096850888867,
4.36205133937433));
#12943=CARTESIAN_POINT('Ctrl Pts',(-6.25181603734438,-0.171382362262575,
4.37293523607869));
#12944=CARTESIAN_POINT('Ctrl Pts',(-6.24105003663889,0.113834567019171,
4.38381579035452));
#12945=CARTESIAN_POINT('Ctrl Pts',(-6.33542564510066,0.383034418620386,
4.39469364740737));
#12946=CARTESIAN_POINT('Ctrl Pts',(-6.55230017515376,0.63552240326747,4.40738028050328));
#12947=CARTESIAN_POINT('Ctrl Pts',(-6.91099640381501,0.784687258636925,
4.4218763046563));
#12948=CARTESIAN_POINT('Ctrl Pts',(-7.34212240019886,0.711207343436876,
4.43817956917959));
#12949=CARTESIAN_POINT('Ctrl Pts',(-7.66784503795017,0.420122820836888,
4.45447719499099));
#12950=CARTESIAN_POINT('Ctrl Pts',(-7.78880772644369,0.000301349021138111,
4.4707704498999));
#12951=CARTESIAN_POINT('Ctrl Pts',(-7.667877587161,-0.419341085827839,4.48705960232271));
#12952=CARTESIAN_POINT('Ctrl Pts',(-7.34230267069937,-0.710297515575184,
4.50334535553822));
#12953=CARTESIAN_POINT('Ctrl Pts',(-6.91190437925101,-0.783412060401462,
4.51962819595119));
#12954=CARTESIAN_POINT('Ctrl Pts',(-6.50863628128277,-0.616365790333621,
4.53590870397414));
#12955=CARTESIAN_POINT('Ctrl Pts',(-6.25607982849799,-0.260409693527577,
4.5521874093325));
#12956=CARTESIAN_POINT('Ctrl Pts',(-6.23161283377708,0.175321606389228,
4.56846487082594));
#12957=CARTESIAN_POINT('Ctrl Pts',(-6.44271176828563,0.557262980844724,
4.58474160682034));
#12958=CARTESIAN_POINT('Ctrl Pts',(-6.82464434492978,0.768358222162331,
4.60101821545767));
#12959=CARTESIAN_POINT('Ctrl Pts',(-7.26037536186215,0.743876395320755,
4.61729512256828));
#12960=CARTESIAN_POINT('Ctrl Pts',(-7.61626704964913,0.491357056997004,
4.63357315010908));
#12961=CARTESIAN_POINT('Ctrl Pts',(-7.78338185515668,0.0880536646158774,
4.64985222966985));
#12962=CARTESIAN_POINT('Ctrl Pts',(-7.72227904989592,-0.270456594079558,
4.66342067449138));
#12963=CARTESIAN_POINT('Ctrl Pts',(-7.56494361675605,-0.505166038725783,
4.67427498609028));
#12964=CARTESIAN_POINT('Ctrl Pts',(-7.34931051926875,-0.687808815183051,
4.68513021846502));
#12965=CARTESIAN_POINT('Ctrl Pts',(-6.99978283745156,-0.788718364067694,
4.69870330867372));
#12966=CARTESIAN_POINT('Ctrl Pts',(-6.58001528872106,-0.667748618933984,
4.71499348628701));
#12967=CARTESIAN_POINT('Ctrl Pts',(-6.28892712013077,-0.342052929566312,
4.7312881611743));
#12968=CARTESIAN_POINT('Ctrl Pts',(-6.21569469059752,0.0887734809755611,
4.74758724186428));
#12969=CARTESIAN_POINT('Ctrl Pts',(-6.38296454904747,0.492623142936048,
4.76389156558651));
#12970=CARTESIAN_POINT('Ctrl Pts',(-6.739578169164,0.745682782278417,4.78020152499504));
#12971=CARTESIAN_POINT('Ctrl Pts',(-7.17633951141972,0.770218713454861,
4.79651776702086));
#12972=CARTESIAN_POINT('Ctrl Pts',(-7.55937071328772,0.558553081416467,
4.81284069537888));
#12973=CARTESIAN_POINT('Ctrl Pts',(-7.77118600830977,0.175328612777807,
4.8291711200582));
#12974=CARTESIAN_POINT('Ctrl Pts',(-7.74663968736165,-0.261977048857528,
4.84550903765717));
#12975=CARTESIAN_POINT('Ctrl Pts',(-7.49310132503884,-0.61959334356644,
4.86185626860575));
#12976=CARTESIAN_POINT('Ctrl Pts',(-7.08792565192062,-0.787152269199519,
4.87821065600015));
#12977=CARTESIAN_POINT('Ctrl Pts',(-6.65545106666535,-0.713968083417749,
4.89457308734717));
#12978=CARTESIAN_POINT('Ctrl Pts',(-6.32807722541735,-0.421152088596462,
4.910946967621));
#12979=CARTESIAN_POINT('Ctrl Pts',(-6.24702100712985,-0.140397334609587,
4.92186764777286));
#12980=CARTESIAN_POINT('Ctrl Pts',(-6.24700200535915,0.000883075965957197,
4.92733213238152));
#12981=CARTESIAN_POINT('Ctrl Pts',(-6.20000025990999,0.00193246945643844,
1.00003735833913));
#12982=CARTESIAN_POINT('Ctrl Pts',(-6.20002044487095,0.15201065585541,1.00584212579936));
#12983=CARTESIAN_POINT('Ctrl Pts',(-6.28611355781982,0.450654413607575,
1.01745595262984));
#12984=CARTESIAN_POINT('Ctrl Pts',(-6.63487773043299,0.762776896374944,
1.0349026678303));
#12985=CARTESIAN_POINT('Ctrl Pts',(-7.09661480461016,0.841046944166038,
1.05237210147879));
#12986=CARTESIAN_POINT('Ctrl Pts',(-7.5301000809641,0.66191148032223,1.06986555847399));
#12987=CARTESIAN_POINT('Ctrl Pts',(-7.8019176387512,0.278705057923738,1.08738232429735));
#12988=CARTESIAN_POINT('Ctrl Pts',(-7.82838413701279,-0.19084760704926,
1.10492270302733));
#12989=CARTESIAN_POINT('Ctrl Pts',(-7.60064075566285,-0.603137091155931,
1.12248646715818));
#12990=CARTESIAN_POINT('Ctrl Pts',(-7.1879122444388,-0.831327694844811,
1.1400736154085));
#12991=CARTESIAN_POINT('Ctrl Pts',(-6.71648331627183,-0.804952825733149,
1.15768402928987));
#12992=CARTESIAN_POINT('Ctrl Pts',(-6.33069129380762,-0.53139586788873,
1.17531762920689));
#12993=CARTESIAN_POINT('Ctrl Pts',(-6.17986938434826,-0.166924530929506,
1.19003152205635));
#12994=CARTESIAN_POINT('Ctrl Pts',(-6.18891827393114,0.139694417819641,
1.20181411747366));
#12995=CARTESIAN_POINT('Ctrl Pts',(-6.28167759636603,0.432287479563812,
1.21360434390419));
#12996=CARTESIAN_POINT('Ctrl Pts',(-6.54498491257115,0.727352514001043,
1.22835639528026));
#12997=CARTESIAN_POINT('Ctrl Pts',(-7.00178799837524,0.858989074734809,
1.2460815491715));
#12998=CARTESIAN_POINT('Ctrl Pts',(-7.45905640505002,0.727341633611197,
1.2638292469814));
#12999=CARTESIAN_POINT('Ctrl Pts',(-7.77665281049733,0.372097321399229,
1.28159932797245));
#13000=CARTESIAN_POINT('Ctrl Pts',(-7.85663990835041,-0.0982374580424732,
1.29939162334549));
#13001=CARTESIAN_POINT('Ctrl Pts',(-7.67391806687674,-0.539592338752092,
1.31720595246947));
#13002=CARTESIAN_POINT('Ctrl Pts',(-7.28390423314539,-0.816419475206943,
1.33504212338853));
#13003=CARTESIAN_POINT('Ctrl Pts',(-6.80581165670056,-0.843349744908527,
1.35289993632842));
#13004=CARTESIAN_POINT('Ctrl Pts',(-6.38616737126169,-0.61151281975725,
1.37077917836497));
#13005=CARTESIAN_POINT('Ctrl Pts',(-6.15391471330266,-0.191448545046746,
1.38867962991899));
#13006=CARTESIAN_POINT('Ctrl Pts',(-6.18078031189829,0.288356063072798,
1.40660105660474));
#13007=CARTESIAN_POINT('Ctrl Pts',(-6.45912099114284,0.680780452257456,
1.42454321935777));
#13008=CARTESIAN_POINT('Ctrl Pts',(-6.90408886634936,0.865172061566579,
1.44250586618275));
#13009=CARTESIAN_POINT('Ctrl Pts',(-7.37948719351768,0.784486199243698,
1.46048873474343));
#13010=CARTESIAN_POINT('Ctrl Pts',(-7.73949168252554,0.462850086060547,
1.47849155669373));
#13011=CARTESIAN_POINT('Ctrl Pts',(-7.87332738631526,-0.0014557841833066,
1.49651404939771));
#13012=CARTESIAN_POINT('Ctrl Pts',(-7.73949699110486,-0.466462821459191,
1.51455592727214));
#13013=CARTESIAN_POINT('Ctrl Pts',(-7.43853082628792,-0.735208997602771,
1.52960672657187));
#13014=CARTESIAN_POINT('Ctrl Pts',(-7.13950426621928,-0.830029799823059,
1.5416567556677));
#13015=CARTESIAN_POINT('Ctrl Pts',(-6.82573429908325,-0.839341203501555,
1.55371299076107));
#13016=CARTESIAN_POINT('Ctrl Pts',(-6.46884268588545,-0.691631510671627,
1.56812451918729));
#13017=CARTESIAN_POINT('Ctrl Pts',(-6.19953260950331,-0.335836989319061,
1.58489796930832));
#13018=CARTESIAN_POINT('Ctrl Pts',(-6.13558329245919,0.087838843174565,
1.60101457637617));
#13019=CARTESIAN_POINT('Ctrl Pts',(-6.28224419701691,0.490989051876738,
1.61714503893002));
#13020=CARTESIAN_POINT('Ctrl Pts',(-6.60413478737033,0.775061465279082,
1.63328911262099));
#13021=CARTESIAN_POINT('Ctrl Pts',(-7.02294084448011,0.870730250827747,
1.64944654818199));
#13022=CARTESIAN_POINT('Ctrl Pts',(-7.43707348216018,0.754258049077075,
1.66561709103637));
#13023=CARTESIAN_POINT('Ctrl Pts',(-7.74477169774561,0.453838654047166,
1.68180048156974));
#13024=CARTESIAN_POINT('Ctrl Pts',(-7.88680288613318,-0.003482702933719,
1.69979600813884));
#13025=CARTESIAN_POINT('Ctrl Pts',(-7.73694295256561,-0.521688074393446,
1.71960864643413));
#13026=CARTESIAN_POINT('Ctrl Pts',(-7.2579246797109,-0.866176668338957,
1.74124367709995));
#13027=CARTESIAN_POINT('Ctrl Pts',(-6.71798257071652,-0.843361624137061,
1.76109465157299));
#13028=CARTESIAN_POINT('Ctrl Pts',(-6.32813840204838,-0.562067108424238,
1.779155502939));
#13029=CARTESIAN_POINT('Ctrl Pts',(-6.1403602470473,-0.172779460138823,
1.79542117132473));
#13030=CARTESIAN_POINT('Ctrl Pts',(-6.16191594592092,0.259681676239064,
1.81169744765855));
#13031=CARTESIAN_POINT('Ctrl Pts',(-6.38773509477738,0.629211178523826,
1.82798403284572));
#13032=CARTESIAN_POINT('Ctrl Pts',(-6.76298297690006,0.845905336791279,
1.84428062449289));
#13033=CARTESIAN_POINT('Ctrl Pts',(-7.1966047520639,0.856877177797125,1.86058691436274));
#13034=CARTESIAN_POINT('Ctrl Pts',(-7.51813159987616,0.691704323104765,
1.87418331464002));
#13035=CARTESIAN_POINT('Ctrl Pts',(-7.70496340534196,0.479537214773933,
1.88506497141452));
#13036=CARTESIAN_POINT('Ctrl Pts',(-7.834243376472,0.228058843588403,1.89594960161061));
#13037=CARTESIAN_POINT('Ctrl Pts',(-7.87040214071621,-0.132058080538115,
1.90956086256863));
#13038=CARTESIAN_POINT('Ctrl Pts',(-7.70176729712619,-0.532544739489079,
1.92590281458038));
#13039=CARTESIAN_POINT('Ctrl Pts',(-7.3617541753632,-0.803795766305812,
1.94225288140178));
#13040=CARTESIAN_POINT('Ctrl Pts',(-6.96910081682361,-0.872691342258758,
1.95724758038991));
#13041=CARTESIAN_POINT('Ctrl Pts',(-6.62358365553027,-0.779878922686934,
1.97088456464667));
#13042=CARTESIAN_POINT('Ctrl Pts',(-6.36438571820951,-0.588772954661729,
1.98316190508021));
#13043=CARTESIAN_POINT('Ctrl Pts',(-6.19306544459119,-0.315928048614165,
1.99544316011942));
#13044=CARTESIAN_POINT('Ctrl Pts',(-6.13303928680132,0.000731296674565001,
2.00772818860116));
#13045=CARTESIAN_POINT('Ctrl Pts',(-6.19306246181983,0.31737131710264,2.02001684693935));
#13046=CARTESIAN_POINT('Ctrl Pts',(-6.36452596264878,0.590662777058206,
2.03230899246722));
#13047=CARTESIAN_POINT('Ctrl Pts',(-6.62407285476001,0.781608449704824,
2.04460448181281));
#13048=CARTESIAN_POINT('Ctrl Pts',(-7.03960726862712,0.894452101215339,
2.06100273047082));
#13049=CARTESIAN_POINT('Ctrl Pts',(-7.58098213708746,0.728278840923384,
2.08150817561209));
#13050=CARTESIAN_POINT('Ctrl Pts',(-7.9216670182819,0.138324035331395,2.10612575173056));
#13051=CARTESIAN_POINT('Ctrl Pts',(-7.77006105183817,-0.525438678362505,
2.13075319116009));
#13052=CARTESIAN_POINT('Ctrl Pts',(-7.20723620509449,-0.909325593088126,
2.15538930422495));
#13053=CARTESIAN_POINT('Ctrl Pts',(-6.53333888373858,-0.807749099412924,
2.18003289797092));
#13054=CARTESIAN_POINT('Ctrl Pts',(-6.1083188432114,-0.274839326778277,
2.204682767912));
#13055=CARTESIAN_POINT('Ctrl Pts',(-6.15924265883207,0.405062095085805,
2.22933770998693));
#13056=CARTESIAN_POINT('Ctrl Pts',(-6.65910391363797,0.868885188693027,
2.25399651054932));
#13057=CARTESIAN_POINT('Ctrl Pts',(-7.34108037988483,0.868897827671466,
2.2786579570982));
#13058=CARTESIAN_POINT('Ctrl Pts',(-7.84103724749041,0.405011680967366,
2.30332083156262));
#13059=CARTESIAN_POINT('Ctrl Pts',(-7.89200269882987,-0.275103355231245,
2.32798391722886));
#13060=CARTESIAN_POINT('Ctrl Pts',(-7.46677961363602,-0.808302976870588,
2.35264599503351));
#13061=CARTESIAN_POINT('Ctrl Pts',(-6.79246102077101,-0.909925026569516,
2.37730584883283));
#13062=CARTESIAN_POINT('Ctrl Pts',(-6.22911235514946,-0.525814889228737,
2.40196226239673));
#13063=CARTESIAN_POINT('Ctrl Pts',(-6.07744456821118,0.138809074175696,
2.42661402385257));
#13064=CARTESIAN_POINT('Ctrl Pts',(-6.41824880300263,0.729027866722014,
2.45125992491537));
#13065=CARTESIAN_POINT('Ctrl Pts',(-7.06934122876124,0.929824149026898,
2.47589876067858));
#13066=CARTESIAN_POINT('Ctrl Pts',(-7.68299796183915,0.634246527935802,
2.50052933613646));
#13067=CARTESIAN_POINT('Ctrl Pts',(-7.93168967879738,0.000445263131447748,
2.52515045678013));
#13068=CARTESIAN_POINT('Ctrl Pts',(-7.68302213647328,-0.633094458923734,
2.54976094441856));
#13069=CARTESIAN_POINT('Ctrl Pts',(-7.07007700890629,-0.928102101680422,
2.57435962067245));
#13070=CARTESIAN_POINT('Ctrl Pts',(-6.42054771123064,-0.727833461900544,
2.59894532553828));
#13071=CARTESIAN_POINT('Ctrl Pts',(-6.08063030273252,-0.138905152375385,
2.62351690334527));
#13072=CARTESIAN_POINT('Ctrl Pts',(-6.20716604633801,0.411896009844242,
2.64398049630671));
#13073=CARTESIAN_POINT('Ctrl Pts',(-6.51199774209192,0.714676452673333,
2.66034317170459));
#13074=CARTESIAN_POINT('Ctrl Pts',(-6.80647130896726,0.843685013671235,
2.67261094147259));
#13075=CARTESIAN_POINT('Ctrl Pts',(-7.12812476587158,0.855502087711664,
2.68487433317324));
#13076=CARTESIAN_POINT('Ctrl Pts',(-7.43161948042588,0.749419002627999,
2.69713320958533));
#13077=CARTESIAN_POINT('Ctrl Pts',(-7.67521904640705,0.539636596661724,
2.7093874343511));
#13078=CARTESIAN_POINT('Ctrl Pts',(-7.82547325176268,0.255576344693996,
2.72163687040038));
#13079=CARTESIAN_POINT('Ctrl Pts',(-7.86123160253771,-0.0635635909156293,
2.73388138286896));
#13080=CARTESIAN_POINT('Ctrl Pts',(-7.76460027897753,-0.425533717492343,
2.74816074914963));
#13081=CARTESIAN_POINT('Ctrl Pts',(-7.47374360660769,-0.751894656156828,
2.76447137187111));
#13082=CARTESIAN_POINT('Ctrl Pts',(-7.00091436223893,-0.88782428734477,
2.78280870439184));
#13083=CARTESIAN_POINT('Ctrl Pts',(-6.52888862282209,-0.751805319722163,
2.80113347394993));
#13084=CARTESIAN_POINT('Ctrl Pts',(-6.2016684053735,-0.385612928895403,
2.81944525307317));
#13085=CARTESIAN_POINT('Ctrl Pts',(-6.11955382035284,0.0981170754742554,
2.83774361225262));
#13086=CARTESIAN_POINT('Ctrl Pts',(-6.30722625617569,0.551073055321834,
2.85602813457377));
#13087=CARTESIAN_POINT('Ctrl Pts',(-6.70680747045044,0.834525970819447,
2.87429840546262));
#13088=CARTESIAN_POINT('Ctrl Pts',(-7.19559869716282,0.861909407171868,
2.8925540164347));
#13089=CARTESIAN_POINT('Ctrl Pts',(-7.62360216624703,0.625277985438662,
2.91079457296321));
#13090=CARTESIAN_POINT('Ctrl Pts',(-7.86012925287909,0.197486531354187,
2.92901967711976));
#13091=CARTESIAN_POINT('Ctrl Pts',(-7.83237012712838,-0.289941720567784,
2.94722894753945));
#13092=CARTESIAN_POINT('Ctrl Pts',(-7.55008001741224,-0.687784692046307,
2.96542200407487));
#13093=CARTESIAN_POINT('Ctrl Pts',(-7.09977586824996,-0.874247976731781,
2.98359847915852));
#13094=CARTESIAN_POINT('Ctrl Pts',(-6.61974323779859,-0.792623075615972,
3.00175800933));
#13095=CARTESIAN_POINT('Ctrl Pts',(-6.257058130519,-0.468413543112272,3.0199002388146));
#13096=CARTESIAN_POINT('Ctrl Pts',(-6.12258713457564,-0.00138700255432796,
3.03802482606703));
#13097=CARTESIAN_POINT('Ctrl Pts',(-6.25706727378645,0.465139317147603,
3.05613142853581));
#13098=CARTESIAN_POINT('Ctrl Pts',(-6.61877666867083,0.788285032559405,
3.07421972093098));
#13099=CARTESIAN_POINT('Ctrl Pts',(-7.09647607914372,0.869376408975484,
3.09228937996591));
#13100=CARTESIAN_POINT('Ctrl Pts',(-7.54362920385282,0.68408153123717,3.11034009649877));
#13101=CARTESIAN_POINT('Ctrl Pts',(-7.82336210739947,0.28970919078182,3.12837156650594));
#13102=CARTESIAN_POINT('Ctrl Pts',(-7.85036951729978,-0.192518648808231,
3.1463834953635));
#13103=CARTESIAN_POINT('Ctrl Pts',(-7.61693284376151,-0.614735291409423,
3.16437560200786));
#13104=CARTESIAN_POINT('Ctrl Pts',(-7.19511476226595,-0.847778676228102,
3.18234760781168));
#13105=CARTESIAN_POINT('Ctrl Pts',(-6.7145098999882,-0.820710857786535,
3.20029925009486));
#13106=CARTESIAN_POINT('Ctrl Pts',(-6.32242256217712,-0.542413764760527,
3.21823027098919));
#13107=CARTESIAN_POINT('Ctrl Pts',(-6.13871066850024,-0.098686345015634,
3.23614042632575));
#13108=CARTESIAN_POINT('Ctrl Pts',(-6.21914065946509,0.374211025419683,
3.25402947870679));
#13109=CARTESIAN_POINT('Ctrl Pts',(-6.53845875539302,0.731406338297415,
3.27189720144838));
#13110=CARTESIAN_POINT('Ctrl Pts',(-6.99831755296742,0.863804065639348,
3.2897433804432));
#13111=CARTESIAN_POINT('Ctrl Pts',(-7.45757029965599,0.731409466469204,
3.30756780748229));
#13112=CARTESIAN_POINT('Ctrl Pts',(-7.77559982146972,0.37540881511312,3.32537028850097));
#13113=CARTESIAN_POINT('Ctrl Pts',(-7.85537931424834,-0.094642652826617,
3.34315063708933));
#13114=CARTESIAN_POINT('Ctrl Pts',(-7.67307624395954,-0.534539169893111,
3.36090867961867));
#13115=CARTESIAN_POINT('Ctrl Pts',(-7.28516805861167,-0.809670332991083,
3.37864425091963));
#13116=CARTESIAN_POINT('Ctrl Pts',(-6.81094328129299,-0.836216654728318,
3.39635719733567));
#13117=CARTESIAN_POINT('Ctrl Pts',(-6.39581795219668,-0.606687244699812,
3.41404737686194));
#13118=CARTESIAN_POINT('Ctrl Pts',(-6.16673282986248,-0.192016386472062,
3.43171465630725));
#13119=CARTESIAN_POINT('Ctrl Pts',(-6.19335105955753,0.280356102113162,
3.44935891493111));
#13120=CARTESIAN_POINT('Ctrl Pts',(-6.46683379484748,0.665660108445628,
3.46698004190314));
#13121=CARTESIAN_POINT('Ctrl Pts',(-6.90284795213186,0.846152102600437,
3.48457793824716));
#13122=CARTESIAN_POINT('Ctrl Pts',(-7.36737219772646,0.767129205800447,
3.50215251490095));
#13123=CARTESIAN_POINT('Ctrl Pts',(-7.71834143496065,0.453434200086869,
3.51970369457236));
#13124=CARTESIAN_POINT('Ctrl Pts',(-7.82645846631761,0.077080609195679,
3.53431012488451));
#13125=CARTESIAN_POINT('Ctrl Pts',(-7.78351602643939,-0.223766099777631,
3.54598350983127));
#13126=CARTESIAN_POINT('Ctrl Pts',(-7.65984666406284,-0.501195016191524,
3.55764904771478));
#13127=CARTESIAN_POINT('Ctrl Pts',(-7.36883520137935,-0.761421141511966,
3.57221624328425));
#13128=CARTESIAN_POINT('Ctrl Pts',(-6.90699782821215,-0.839986918687281,
3.58967328199228));
#13129=CARTESIAN_POINT('Ctrl Pts',(-6.5235772119384,-0.680444831465126,
3.60516965595896));
#13130=CARTESIAN_POINT('Ctrl Pts',(-6.29205860881578,-0.410854643842501,
3.6187136684483));
#13131=CARTESIAN_POINT('Ctrl Pts',(-6.19144251696091,-0.123792268925567,
3.63031232027941));
#13132=CARTESIAN_POINT('Ctrl Pts',(-6.20295651325157,0.179997595512823,
3.64190047202365));
#13133=CARTESIAN_POINT('Ctrl Pts',(-6.32432621115477,0.458374743512086,
3.65347812777622));
#13134=CARTESIAN_POINT('Ctrl Pts',(-6.53898438351643,0.672840241042802,
3.66504529364933));
#13135=CARTESIAN_POINT('Ctrl Pts',(-6.81680637706894,0.794134031701534,
3.67660197812095));
#13136=CARTESIAN_POINT('Ctrl Pts',(-7.11950248291682,0.805397533837699,
3.68814819174188));
#13137=CARTESIAN_POINT('Ctrl Pts',(-7.34163561569263,0.727628486768507,
3.69712044609008));
#13138=CARTESIAN_POINT('Ctrl Pts',(-7.53458281141515,0.599570945127131,
3.70608728556614));
#13139=CARTESIAN_POINT('Ctrl Pts',(-7.71503532521363,0.400461841999,3.71632891696956));
#13140=CARTESIAN_POINT('Ctrl Pts',(-7.82528743114405,0.0430926937144543,
3.73039630239659));
#13141=CARTESIAN_POINT('Ctrl Pts',(-7.74111169379658,-0.37323537543407,
3.74636272256909));
#13142=CARTESIAN_POINT('Ctrl Pts',(-7.44499573228645,-0.704767123835098,
3.76294659713056));
#13143=CARTESIAN_POINT('Ctrl Pts',(-7.00172600054551,-0.832350159693755,
3.78014508956006));
#13144=CARTESIAN_POINT('Ctrl Pts',(-6.55926311085665,-0.704755991680177,
3.79732045846001));
#13145=CARTESIAN_POINT('Ctrl Pts',(-6.2528315275211,-0.361772892660608,
3.81447281592693));
#13146=CARTESIAN_POINT('Ctrl Pts',(-6.17601189131465,0.0911409447444953,
3.83160228337755));
#13147=CARTESIAN_POINT('Ctrl Pts',(-6.35159897954253,0.514776986788965,
3.84870899394101));
#13148=CARTESIAN_POINT('Ctrl Pts',(-6.72535286944806,0.780122083208515,
3.86579309179979));
#13149=CARTESIAN_POINT('Ctrl Pts',(-7.13122870473182,0.802254155922275,
3.88095899359145));
#13150=CARTESIAN_POINT('Ctrl Pts',(-7.44985202071078,0.662844517922881,
3.89421470788503));
#13151=CARTESIAN_POINT('Ctrl Pts',(-7.66049480984587,0.452421922662202,
3.90556689264628));
#13152=CARTESIAN_POINT('Ctrl Pts',(-7.77936222711058,0.179641079514188,
3.91690927461427));
#13153=CARTESIAN_POINT('Ctrl Pts',(-7.79055864897702,-0.117447939280878,
3.92824190893221));
#13154=CARTESIAN_POINT('Ctrl Pts',(-7.69235883457516,-0.397692735498425,
3.93956485365948));
#13155=CARTESIAN_POINT('Ctrl Pts',(-7.4988193112063,-0.622862064421365,
3.95087816922642));
#13156=CARTESIAN_POINT('Ctrl Pts',(-7.23669309425985,-0.760857052520071,
3.96218191668704));
#13157=CARTESIAN_POINT('Ctrl Pts',(-6.84397122474983,-0.806385392143749,
3.97724090685452));
#13158=CARTESIAN_POINT('Ctrl Pts',(-6.3759149329141,-0.581575494059258,
3.99604104936904));
#13159=CARTESIAN_POINT('Ctrl Pts',(-6.14801487092373,-0.00140577011587543,
4.01856401164168));
#13160=CARTESIAN_POINT('Ctrl Pts',(-6.37569406553146,0.577216837917985,
4.04105035155356));
#13161=CARTESIAN_POINT('Ctrl Pts',(-6.93503804704956,0.846504117962824,
4.06350067666592));
#13162=CARTESIAN_POINT('Ctrl Pts',(-7.52735353249786,0.663517124905538,
4.08591563261074));
#13163=CARTESIAN_POINT('Ctrl Pts',(-7.83667549320556,0.127633503183688,
4.10829588960443));
#13164=CARTESIAN_POINT('Ctrl Pts',(-7.69892862810743,-0.475216209100622,
4.13064214875721));
#13165=CARTESIAN_POINT('Ctrl Pts',(-7.24587822138796,-0.783213519985818,
4.15047591997482));
#13166=CARTESIAN_POINT('Ctrl Pts',(-6.78448909503242,-0.770150049272615,
4.16780939837816));
#13167=CARTESIAN_POINT('Ctrl Pts',(-6.44291255401028,-0.573358437418835,
4.18265244830762));
#13168=CARTESIAN_POINT('Ctrl Pts',(-6.23727444607057,-0.236582538920206,
4.19748151807985));
#13169=CARTESIAN_POINT('Ctrl Pts',(-6.21750233201011,0.156779347523281,
4.21229685032696));
#13170=CARTESIAN_POINT('Ctrl Pts',(-6.38851989967645,0.511421035774412,
4.22709868951428));
#13171=CARTESIAN_POINT('Ctrl Pts',(-6.68127276436824,0.721655369840554,
4.24065490665371));
#13172=CARTESIAN_POINT('Ctrl Pts',(-6.99873870462004,0.781500222137114,
4.25296927229394));
#13173=CARTESIAN_POINT('Ctrl Pts',(-7.28423799128053,0.727580241858167,
4.26404501085876));
#13174=CARTESIAN_POINT('Ctrl Pts',(-7.52996735384668,0.573044604556925,
4.27511366794562));
#13175=CARTESIAN_POINT('Ctrl Pts',(-7.70249233600175,0.339504000304913,
4.28617535676904));
#13176=CARTESIAN_POINT('Ctrl Pts',(-7.77704029199075,0.0596812865399207,
4.29723019232866));
#13177=CARTESIAN_POINT('Ctrl Pts',(-7.73493077249201,-0.32516426809182,
4.31196099263524));
#13178=CARTESIAN_POINT('Ctrl Pts',(-7.48195320169677,-0.642258532616097,
4.32667855077855));
#13179=CARTESIAN_POINT('Ctrl Pts',(-7.11676447072565,-0.768672906025829,
4.34138335007881));
#13180=CARTESIAN_POINT('Ctrl Pts',(-6.82822052968084,-0.75826459078673,
4.35240569057047));
#13181=CARTESIAN_POINT('Ctrl Pts',(-6.56324655367934,-0.642480501470498,
4.36342189483669));
#13182=CARTESIAN_POINT('Ctrl Pts',(-6.3590246126422,-0.438361948172784,
4.37443208856579));
#13183=CARTESIAN_POINT('Ctrl Pts',(-6.24366823031993,-0.173725992278803,
4.38543639651659));
#13184=CARTESIAN_POINT('Ctrl Pts',(-6.23278862096309,0.114603786226641,
4.39643494391794));
#13185=CARTESIAN_POINT('Ctrl Pts',(-6.32818140570146,0.3866727001158,4.40742785948479));
#13186=CARTESIAN_POINT('Ctrl Pts',(-6.54732728408833,0.641795528726263,
4.42024651101618));
#13187=CARTESIAN_POINT('Ctrl Pts',(-6.90966296029133,0.792450205988824,
4.43488744119146));
#13188=CARTESIAN_POINT('Ctrl Pts',(-7.34497884959273,0.718229352606656,
4.45134684847234));
#13189=CARTESIAN_POINT('Ctrl Pts',(-7.67373744220819,0.42439860304808,4.46779506017063));
#13190=CARTESIAN_POINT('Ctrl Pts',(-7.7957623026863,0.000795392209376382,
4.48423253597012));
#13191=CARTESIAN_POINT('Ctrl Pts',(-7.6737681501059,-0.422451523433032,
4.50065973137187));
#13192=CARTESIAN_POINT('Ctrl Pts',(-7.34550270887416,-0.715780174479536,
4.51707711746896));
#13193=CARTESIAN_POINT('Ctrl Pts',(-6.91173568096419,-0.789442989854855,
4.53348515869499));
#13194=CARTESIAN_POINT('Ctrl Pts',(-6.50548543634235,-0.62113576023861,
4.54988433137086));
#13195=CARTESIAN_POINT('Ctrl Pts',(-6.25117725190974,-0.26266942709969,
4.56627511486019));
#13196=CARTESIAN_POINT('Ctrl Pts',(-6.22657268391725,0.175941615799059,
4.58265798957595));
#13197=CARTESIAN_POINT('Ctrl Pts',(-6.43900037753832,0.560237327905976,
4.59903344336352));
#13198=CARTESIAN_POINT('Ctrl Pts',(-6.82315231070266,0.772532064615231,
4.61540196293227));
#13199=CARTESIAN_POINT('Ctrl Pts',(-7.2612181287951,0.747894614274433,4.63176404577646));
#13200=CARTESIAN_POINT('Ctrl Pts',(-7.61885424416052,0.494109349486934,
4.64812018315545));
#13201=CARTESIAN_POINT('Ctrl Pts',(-7.78669901230814,0.0889725746862699,
4.66447087596232));
#13202=CARTESIAN_POINT('Ctrl Pts',(-7.72532501848925,-0.270994143806812,
4.67809233336064));
#13203=CARTESIAN_POINT('Ctrl Pts',(-7.56738721688822,-0.506594326857297,
4.68898728035258));
#13204=CARTESIAN_POINT('Ctrl Pts',(-7.35097564028756,-0.689891456361417,
4.69988083117445));
#13205=CARTESIAN_POINT('Ctrl Pts',(-7.0003169174225,-0.79110738140522,4.71349530909451));
#13206=CARTESIAN_POINT('Ctrl Pts',(-6.57937611771461,-0.669773743535281,
4.72982925479887));
#13207=CARTESIAN_POINT('Ctrl Pts',(-6.28761734218788,-0.343284450620702,
4.74616028288309));
#13208=CARTESIAN_POINT('Ctrl Pts',(-6.21426971041073,0.0883871334668474,
4.76248890194073));
#13209=CARTESIAN_POINT('Ctrl Pts',(-6.38182100128212,0.492840639406237,
4.77881561989744));
#13210=CARTESIAN_POINT('Ctrl Pts',(-6.73884045313308,0.746153973023737,
4.79514095601288));
#13211=CARTESIAN_POINT('Ctrl Pts',(-7.17589338359863,0.770679755263529,
4.81146540426486));
#13212=CARTESIAN_POINT('Ctrl Pts',(-7.55900114520461,0.55894423669953,4.82778951061359));
#13213=CARTESIAN_POINT('Ctrl Pts',(-7.77075750409873,0.175788412965931,
4.84411370102291));
#13214=CARTESIAN_POINT('Ctrl Pts',(-7.74620736592161,-0.261233995076225,
4.86043866853608));
#13215=CARTESIAN_POINT('Ctrl Pts',(-7.49294321470503,-0.618448872812403,
4.87676449790797));
#13216=CARTESIAN_POINT('Ctrl Pts',(-7.08837163954946,-0.785730122461179,
4.89309260172666));
#13217=CARTESIAN_POINT('Ctrl Pts',(-6.65674407499508,-0.712671607108413,
4.90942182102584));
#13218=CARTESIAN_POINT('Ctrl Pts',(-6.33017289353631,-0.420518596063947,
4.92575590410514));
#13219=CARTESIAN_POINT('Ctrl Pts',(-6.2493887150478,-0.140566474730618,
4.93664355063335));
#13220=CARTESIAN_POINT('Ctrl Pts',(-6.24936976727053,0.000312488344807942,
4.94209250793942));
#13221=CARTESIAN_POINT('',(-6.20000025990999,0.00193246945643844,1.00003735833913));
#13222=CARTESIAN_POINT('Origin',(-6.2,-1.64817900953001E-18,1.05));
#13223=CARTESIAN_POINT('',(-6.24936976727053,0.000312488344807943,4.94209250793942));
#13224=CARTESIAN_POINT('Ctrl Pts',(-6.20000025990999,0.00193246945643844,
1.00003735833913));
#13225=CARTESIAN_POINT('Ctrl Pts',(-6.20002044487095,0.15201065585541,1.00584212579936));
#13226=CARTESIAN_POINT('Ctrl Pts',(-6.28611355781982,0.450654413607575,
1.01745595262984));
#13227=CARTESIAN_POINT('Ctrl Pts',(-6.63487773043299,0.762776896374944,
1.0349026678303));
#13228=CARTESIAN_POINT('Ctrl Pts',(-7.09661480461016,0.841046944166038,
1.05237210147879));
#13229=CARTESIAN_POINT('Ctrl Pts',(-7.5301000809641,0.66191148032223,1.06986555847399));
#13230=CARTESIAN_POINT('Ctrl Pts',(-7.8019176387512,0.278705057923738,1.08738232429735));
#13231=CARTESIAN_POINT('Ctrl Pts',(-7.82838413701279,-0.19084760704926,
1.10492270302733));
#13232=CARTESIAN_POINT('Ctrl Pts',(-7.60064075566285,-0.603137091155931,
1.12248646715818));
#13233=CARTESIAN_POINT('Ctrl Pts',(-7.1879122444388,-0.831327694844811,
1.1400736154085));
#13234=CARTESIAN_POINT('Ctrl Pts',(-6.71648331627183,-0.804952825733149,
1.15768402928987));
#13235=CARTESIAN_POINT('Ctrl Pts',(-6.33069129380762,-0.53139586788873,
1.17531762920689));
#13236=CARTESIAN_POINT('Ctrl Pts',(-6.17986938434826,-0.166924530929506,
1.19003152205635));
#13237=CARTESIAN_POINT('Ctrl Pts',(-6.18891827393114,0.139694417819641,
1.20181411747366));
#13238=CARTESIAN_POINT('Ctrl Pts',(-6.28167759636603,0.432287479563812,
1.21360434390419));
#13239=CARTESIAN_POINT('Ctrl Pts',(-6.54498491257115,0.727352514001043,
1.22835639528026));
#13240=CARTESIAN_POINT('Ctrl Pts',(-7.00178799837524,0.858989074734809,
1.2460815491715));
#13241=CARTESIAN_POINT('Ctrl Pts',(-7.45905640505002,0.727341633611197,
1.2638292469814));
#13242=CARTESIAN_POINT('Ctrl Pts',(-7.77665281049733,0.372097321399229,
1.28159932797245));
#13243=CARTESIAN_POINT('Ctrl Pts',(-7.85663990835041,-0.0982374580424732,
1.29939162334549));
#13244=CARTESIAN_POINT('Ctrl Pts',(-7.67391806687674,-0.539592338752092,
1.31720595246947));
#13245=CARTESIAN_POINT('Ctrl Pts',(-7.28390423314539,-0.816419475206943,
1.33504212338853));
#13246=CARTESIAN_POINT('Ctrl Pts',(-6.80581165670056,-0.843349744908527,
1.35289993632842));
#13247=CARTESIAN_POINT('Ctrl Pts',(-6.38616737126169,-0.61151281975725,
1.37077917836497));
#13248=CARTESIAN_POINT('Ctrl Pts',(-6.15391471330266,-0.191448545046746,
1.38867962991899));
#13249=CARTESIAN_POINT('Ctrl Pts',(-6.18078031189829,0.288356063072798,
1.40660105660474));
#13250=CARTESIAN_POINT('Ctrl Pts',(-6.45912099114284,0.680780452257456,
1.42454321935777));
#13251=CARTESIAN_POINT('Ctrl Pts',(-6.90408886634936,0.865172061566579,
1.44250586618275));
#13252=CARTESIAN_POINT('Ctrl Pts',(-7.37948719351768,0.784486199243698,
1.46048873474343));
#13253=CARTESIAN_POINT('Ctrl Pts',(-7.73949168252554,0.462850086060547,
1.47849155669373));
#13254=CARTESIAN_POINT('Ctrl Pts',(-7.87332738631526,-0.0014557841833066,
1.49651404939771));
#13255=CARTESIAN_POINT('Ctrl Pts',(-7.73949699110486,-0.466462821459191,
1.51455592727214));
#13256=CARTESIAN_POINT('Ctrl Pts',(-7.43853082628792,-0.735208997602771,
1.52960672657187));
#13257=CARTESIAN_POINT('Ctrl Pts',(-7.13950426621928,-0.830029799823059,
1.5416567556677));
#13258=CARTESIAN_POINT('Ctrl Pts',(-6.82573429908325,-0.839341203501555,
1.55371299076107));
#13259=CARTESIAN_POINT('Ctrl Pts',(-6.46884268588545,-0.691631510671627,
1.56812451918729));
#13260=CARTESIAN_POINT('Ctrl Pts',(-6.19953260950331,-0.335836989319061,
1.58489796930832));
#13261=CARTESIAN_POINT('Ctrl Pts',(-6.13558329245919,0.087838843174565,
1.60101457637617));
#13262=CARTESIAN_POINT('Ctrl Pts',(-6.28224419701691,0.490989051876738,
1.61714503893002));
#13263=CARTESIAN_POINT('Ctrl Pts',(-6.60413478737033,0.775061465279082,
1.63328911262099));
#13264=CARTESIAN_POINT('Ctrl Pts',(-7.02294084448011,0.870730250827747,
1.64944654818199));
#13265=CARTESIAN_POINT('Ctrl Pts',(-7.43707348216018,0.754258049077075,
1.66561709103637));
#13266=CARTESIAN_POINT('Ctrl Pts',(-7.74477169774561,0.453838654047166,
1.68180048156974));
#13267=CARTESIAN_POINT('Ctrl Pts',(-7.88680288613318,-0.003482702933719,
1.69979600813884));
#13268=CARTESIAN_POINT('Ctrl Pts',(-7.73694295256561,-0.521688074393446,
1.71960864643413));
#13269=CARTESIAN_POINT('Ctrl Pts',(-7.2579246797109,-0.866176668338957,
1.74124367709995));
#13270=CARTESIAN_POINT('Ctrl Pts',(-6.71798257071652,-0.843361624137061,
1.76109465157299));
#13271=CARTESIAN_POINT('Ctrl Pts',(-6.32813840204838,-0.562067108424238,
1.779155502939));
#13272=CARTESIAN_POINT('Ctrl Pts',(-6.1403602470473,-0.172779460138823,
1.79542117132473));
#13273=CARTESIAN_POINT('Ctrl Pts',(-6.16191594592092,0.259681676239064,
1.81169744765855));
#13274=CARTESIAN_POINT('Ctrl Pts',(-6.38773509477738,0.629211178523826,
1.82798403284572));
#13275=CARTESIAN_POINT('Ctrl Pts',(-6.76298297690006,0.845905336791279,
1.84428062449289));
#13276=CARTESIAN_POINT('Ctrl Pts',(-7.1966047520639,0.856877177797125,1.86058691436274));
#13277=CARTESIAN_POINT('Ctrl Pts',(-7.51813159987616,0.691704323104765,
1.87418331464002));
#13278=CARTESIAN_POINT('Ctrl Pts',(-7.70496340534196,0.479537214773933,
1.88506497141452));
#13279=CARTESIAN_POINT('Ctrl Pts',(-7.834243376472,0.228058843588403,1.89594960161061));
#13280=CARTESIAN_POINT('Ctrl Pts',(-7.87040214071621,-0.132058080538115,
1.90956086256863));
#13281=CARTESIAN_POINT('Ctrl Pts',(-7.70176729712619,-0.532544739489079,
1.92590281458038));
#13282=CARTESIAN_POINT('Ctrl Pts',(-7.3617541753632,-0.803795766305812,
1.94225288140178));
#13283=CARTESIAN_POINT('Ctrl Pts',(-6.96910081682361,-0.872691342258758,
1.95724758038991));
#13284=CARTESIAN_POINT('Ctrl Pts',(-6.62358365553027,-0.779878922686934,
1.97088456464667));
#13285=CARTESIAN_POINT('Ctrl Pts',(-6.36438571820951,-0.588772954661729,
1.98316190508021));
#13286=CARTESIAN_POINT('Ctrl Pts',(-6.19306544459119,-0.315928048614165,
1.99544316011942));
#13287=CARTESIAN_POINT('Ctrl Pts',(-6.13303928680132,0.000731296674565001,
2.00772818860116));
#13288=CARTESIAN_POINT('Ctrl Pts',(-6.19306246181983,0.31737131710264,2.02001684693935));
#13289=CARTESIAN_POINT('Ctrl Pts',(-6.36452596264878,0.590662777058206,
2.03230899246722));
#13290=CARTESIAN_POINT('Ctrl Pts',(-6.62407285476001,0.781608449704824,
2.04460448181281));
#13291=CARTESIAN_POINT('Ctrl Pts',(-7.03960726862712,0.894452101215339,
2.06100273047082));
#13292=CARTESIAN_POINT('Ctrl Pts',(-7.58098213708746,0.728278840923384,
2.08150817561209));
#13293=CARTESIAN_POINT('Ctrl Pts',(-7.9216670182819,0.138324035331395,2.10612575173056));
#13294=CARTESIAN_POINT('Ctrl Pts',(-7.77006105183817,-0.525438678362505,
2.13075319116009));
#13295=CARTESIAN_POINT('Ctrl Pts',(-7.20723620509449,-0.909325593088126,
2.15538930422495));
#13296=CARTESIAN_POINT('Ctrl Pts',(-6.53333888373858,-0.807749099412924,
2.18003289797092));
#13297=CARTESIAN_POINT('Ctrl Pts',(-6.1083188432114,-0.274839326778277,
2.204682767912));
#13298=CARTESIAN_POINT('Ctrl Pts',(-6.15924265883207,0.405062095085805,
2.22933770998693));
#13299=CARTESIAN_POINT('Ctrl Pts',(-6.65910391363797,0.868885188693027,
2.25399651054932));
#13300=CARTESIAN_POINT('Ctrl Pts',(-7.34108037988483,0.868897827671466,
2.2786579570982));
#13301=CARTESIAN_POINT('Ctrl Pts',(-7.84103724749041,0.405011680967366,
2.30332083156262));
#13302=CARTESIAN_POINT('Ctrl Pts',(-7.89200269882987,-0.275103355231245,
2.32798391722886));
#13303=CARTESIAN_POINT('Ctrl Pts',(-7.46677961363602,-0.808302976870588,
2.35264599503351));
#13304=CARTESIAN_POINT('Ctrl Pts',(-6.79246102077101,-0.909925026569516,
2.37730584883283));
#13305=CARTESIAN_POINT('Ctrl Pts',(-6.22911235514946,-0.525814889228737,
2.40196226239673));
#13306=CARTESIAN_POINT('Ctrl Pts',(-6.07744456821118,0.138809074175696,
2.42661402385257));
#13307=CARTESIAN_POINT('Ctrl Pts',(-6.41824880300263,0.729027866722014,
2.45125992491537));
#13308=CARTESIAN_POINT('Ctrl Pts',(-7.06934122876124,0.929824149026898,
2.47589876067858));
#13309=CARTESIAN_POINT('Ctrl Pts',(-7.68299796183915,0.634246527935802,
2.50052933613646));
#13310=CARTESIAN_POINT('Ctrl Pts',(-7.93168967879738,0.000445263131447748,
2.52515045678013));
#13311=CARTESIAN_POINT('Ctrl Pts',(-7.68302213647328,-0.633094458923734,
2.54976094441856));
#13312=CARTESIAN_POINT('Ctrl Pts',(-7.07007700890629,-0.928102101680422,
2.57435962067245));
#13313=CARTESIAN_POINT('Ctrl Pts',(-6.42054771123064,-0.727833461900544,
2.59894532553828));
#13314=CARTESIAN_POINT('Ctrl Pts',(-6.08063030273252,-0.138905152375385,
2.62351690334527));
#13315=CARTESIAN_POINT('Ctrl Pts',(-6.20716604633801,0.411896009844242,
2.64398049630671));
#13316=CARTESIAN_POINT('Ctrl Pts',(-6.51199774209192,0.714676452673333,
2.66034317170459));
#13317=CARTESIAN_POINT('Ctrl Pts',(-6.80647130896726,0.843685013671235,
2.67261094147259));
#13318=CARTESIAN_POINT('Ctrl Pts',(-7.12812476587158,0.855502087711664,
2.68487433317324));
#13319=CARTESIAN_POINT('Ctrl Pts',(-7.43161948042588,0.749419002627999,
2.69713320958533));
#13320=CARTESIAN_POINT('Ctrl Pts',(-7.67521904640705,0.539636596661724,
2.7093874343511));
#13321=CARTESIAN_POINT('Ctrl Pts',(-7.82547325176268,0.255576344693996,
2.72163687040038));
#13322=CARTESIAN_POINT('Ctrl Pts',(-7.86123160253771,-0.0635635909156293,
2.73388138286896));
#13323=CARTESIAN_POINT('Ctrl Pts',(-7.76460027897753,-0.425533717492343,
2.74816074914963));
#13324=CARTESIAN_POINT('Ctrl Pts',(-7.47374360660769,-0.751894656156828,
2.76447137187111));
#13325=CARTESIAN_POINT('Ctrl Pts',(-7.00091436223893,-0.88782428734477,
2.78280870439184));
#13326=CARTESIAN_POINT('Ctrl Pts',(-6.52888862282209,-0.751805319722163,
2.80113347394993));
#13327=CARTESIAN_POINT('Ctrl Pts',(-6.2016684053735,-0.385612928895403,
2.81944525307317));
#13328=CARTESIAN_POINT('Ctrl Pts',(-6.11955382035284,0.0981170754742554,
2.83774361225262));
#13329=CARTESIAN_POINT('Ctrl Pts',(-6.30722625617569,0.551073055321834,
2.85602813457377));
#13330=CARTESIAN_POINT('Ctrl Pts',(-6.70680747045044,0.834525970819447,
2.87429840546262));
#13331=CARTESIAN_POINT('Ctrl Pts',(-7.19559869716282,0.861909407171868,
2.8925540164347));
#13332=CARTESIAN_POINT('Ctrl Pts',(-7.62360216624703,0.625277985438662,
2.91079457296321));
#13333=CARTESIAN_POINT('Ctrl Pts',(-7.86012925287909,0.197486531354187,
2.92901967711976));
#13334=CARTESIAN_POINT('Ctrl Pts',(-7.83237012712838,-0.289941720567784,
2.94722894753945));
#13335=CARTESIAN_POINT('Ctrl Pts',(-7.55008001741224,-0.687784692046307,
2.96542200407487));
#13336=CARTESIAN_POINT('Ctrl Pts',(-7.09977586824996,-0.874247976731781,
2.98359847915852));
#13337=CARTESIAN_POINT('Ctrl Pts',(-6.61974323779859,-0.792623075615972,
3.00175800933));
#13338=CARTESIAN_POINT('Ctrl Pts',(-6.257058130519,-0.468413543112272,3.0199002388146));
#13339=CARTESIAN_POINT('Ctrl Pts',(-6.12258713457564,-0.00138700255432796,
3.03802482606703));
#13340=CARTESIAN_POINT('Ctrl Pts',(-6.25706727378645,0.465139317147603,
3.05613142853581));
#13341=CARTESIAN_POINT('Ctrl Pts',(-6.61877666867083,0.788285032559405,
3.07421972093098));
#13342=CARTESIAN_POINT('Ctrl Pts',(-7.09647607914372,0.869376408975484,
3.09228937996591));
#13343=CARTESIAN_POINT('Ctrl Pts',(-7.54362920385282,0.68408153123717,3.11034009649877));
#13344=CARTESIAN_POINT('Ctrl Pts',(-7.82336210739947,0.28970919078182,3.12837156650594));
#13345=CARTESIAN_POINT('Ctrl Pts',(-7.85036951729978,-0.192518648808231,
3.1463834953635));
#13346=CARTESIAN_POINT('Ctrl Pts',(-7.61693284376151,-0.614735291409423,
3.16437560200786));
#13347=CARTESIAN_POINT('Ctrl Pts',(-7.19511476226595,-0.847778676228102,
3.18234760781168));
#13348=CARTESIAN_POINT('Ctrl Pts',(-6.7145098999882,-0.820710857786535,
3.20029925009486));
#13349=CARTESIAN_POINT('Ctrl Pts',(-6.32242256217712,-0.542413764760527,
3.21823027098919));
#13350=CARTESIAN_POINT('Ctrl Pts',(-6.13871066850024,-0.098686345015634,
3.23614042632575));
#13351=CARTESIAN_POINT('Ctrl Pts',(-6.21914065946509,0.374211025419683,
3.25402947870679));
#13352=CARTESIAN_POINT('Ctrl Pts',(-6.53845875539302,0.731406338297415,
3.27189720144838));
#13353=CARTESIAN_POINT('Ctrl Pts',(-6.99831755296742,0.863804065639348,
3.2897433804432));
#13354=CARTESIAN_POINT('Ctrl Pts',(-7.45757029965599,0.731409466469204,
3.30756780748229));
#13355=CARTESIAN_POINT('Ctrl Pts',(-7.77559982146972,0.37540881511312,3.32537028850097));
#13356=CARTESIAN_POINT('Ctrl Pts',(-7.85537931424834,-0.094642652826617,
3.34315063708933));
#13357=CARTESIAN_POINT('Ctrl Pts',(-7.67307624395954,-0.534539169893111,
3.36090867961867));
#13358=CARTESIAN_POINT('Ctrl Pts',(-7.28516805861167,-0.809670332991083,
3.37864425091963));
#13359=CARTESIAN_POINT('Ctrl Pts',(-6.81094328129299,-0.836216654728318,
3.39635719733567));
#13360=CARTESIAN_POINT('Ctrl Pts',(-6.39581795219668,-0.606687244699812,
3.41404737686194));
#13361=CARTESIAN_POINT('Ctrl Pts',(-6.16673282986248,-0.192016386472062,
3.43171465630725));
#13362=CARTESIAN_POINT('Ctrl Pts',(-6.19335105955753,0.280356102113162,
3.44935891493111));
#13363=CARTESIAN_POINT('Ctrl Pts',(-6.46683379484748,0.665660108445628,
3.46698004190314));
#13364=CARTESIAN_POINT('Ctrl Pts',(-6.90284795213186,0.846152102600437,
3.48457793824716));
#13365=CARTESIAN_POINT('Ctrl Pts',(-7.36737219772646,0.767129205800447,
3.50215251490095));
#13366=CARTESIAN_POINT('Ctrl Pts',(-7.71834143496065,0.453434200086869,
3.51970369457236));
#13367=CARTESIAN_POINT('Ctrl Pts',(-7.82645846631761,0.077080609195679,
3.53431012488451));
#13368=CARTESIAN_POINT('Ctrl Pts',(-7.78351602643939,-0.223766099777631,
3.54598350983127));
#13369=CARTESIAN_POINT('Ctrl Pts',(-7.65984666406284,-0.501195016191524,
3.55764904771478));
#13370=CARTESIAN_POINT('Ctrl Pts',(-7.36883520137935,-0.761421141511966,
3.57221624328425));
#13371=CARTESIAN_POINT('Ctrl Pts',(-6.90699782821215,-0.839986918687281,
3.58967328199228));
#13372=CARTESIAN_POINT('Ctrl Pts',(-6.5235772119384,-0.680444831465126,
3.60516965595896));
#13373=CARTESIAN_POINT('Ctrl Pts',(-6.29205860881578,-0.410854643842501,
3.6187136684483));
#13374=CARTESIAN_POINT('Ctrl Pts',(-6.19144251696091,-0.123792268925567,
3.63031232027941));
#13375=CARTESIAN_POINT('Ctrl Pts',(-6.20295651325157,0.179997595512823,
3.64190047202365));
#13376=CARTESIAN_POINT('Ctrl Pts',(-6.32432621115477,0.458374743512086,
3.65347812777622));
#13377=CARTESIAN_POINT('Ctrl Pts',(-6.53898438351643,0.672840241042802,
3.66504529364933));
#13378=CARTESIAN_POINT('Ctrl Pts',(-6.81680637706894,0.794134031701534,
3.67660197812095));
#13379=CARTESIAN_POINT('Ctrl Pts',(-7.11950248291682,0.805397533837699,
3.68814819174188));
#13380=CARTESIAN_POINT('Ctrl Pts',(-7.34163561569263,0.727628486768507,
3.69712044609008));
#13381=CARTESIAN_POINT('Ctrl Pts',(-7.53458281141515,0.599570945127131,
3.70608728556614));
#13382=CARTESIAN_POINT('Ctrl Pts',(-7.71503532521363,0.400461841999,3.71632891696956));
#13383=CARTESIAN_POINT('Ctrl Pts',(-7.82528743114405,0.0430926937144543,
3.73039630239659));
#13384=CARTESIAN_POINT('Ctrl Pts',(-7.74111169379658,-0.37323537543407,
3.74636272256909));
#13385=CARTESIAN_POINT('Ctrl Pts',(-7.44499573228645,-0.704767123835098,
3.76294659713056));
#13386=CARTESIAN_POINT('Ctrl Pts',(-7.00172600054551,-0.832350159693755,
3.78014508956006));
#13387=CARTESIAN_POINT('Ctrl Pts',(-6.55926311085665,-0.704755991680177,
3.79732045846001));
#13388=CARTESIAN_POINT('Ctrl Pts',(-6.2528315275211,-0.361772892660608,
3.81447281592693));
#13389=CARTESIAN_POINT('Ctrl Pts',(-6.17601189131465,0.0911409447444953,
3.83160228337755));
#13390=CARTESIAN_POINT('Ctrl Pts',(-6.35159897954253,0.514776986788965,
3.84870899394101));
#13391=CARTESIAN_POINT('Ctrl Pts',(-6.72535286944806,0.780122083208515,
3.86579309179979));
#13392=CARTESIAN_POINT('Ctrl Pts',(-7.13122870473182,0.802254155922275,
3.88095899359145));
#13393=CARTESIAN_POINT('Ctrl Pts',(-7.44985202071078,0.662844517922881,
3.89421470788503));
#13394=CARTESIAN_POINT('Ctrl Pts',(-7.66049480984587,0.452421922662202,
3.90556689264628));
#13395=CARTESIAN_POINT('Ctrl Pts',(-7.77936222711058,0.179641079514188,
3.91690927461427));
#13396=CARTESIAN_POINT('Ctrl Pts',(-7.79055864897702,-0.117447939280878,
3.92824190893221));
#13397=CARTESIAN_POINT('Ctrl Pts',(-7.69235883457516,-0.397692735498425,
3.93956485365948));
#13398=CARTESIAN_POINT('Ctrl Pts',(-7.4988193112063,-0.622862064421365,
3.95087816922642));
#13399=CARTESIAN_POINT('Ctrl Pts',(-7.23669309425985,-0.760857052520071,
3.96218191668704));
#13400=CARTESIAN_POINT('Ctrl Pts',(-6.84397122474983,-0.806385392143749,
3.97724090685452));
#13401=CARTESIAN_POINT('Ctrl Pts',(-6.3759149329141,-0.581575494059258,
3.99604104936904));
#13402=CARTESIAN_POINT('Ctrl Pts',(-6.14801487092373,-0.00140577011587543,
4.01856401164168));
#13403=CARTESIAN_POINT('Ctrl Pts',(-6.37569406553146,0.577216837917985,
4.04105035155356));
#13404=CARTESIAN_POINT('Ctrl Pts',(-6.93503804704956,0.846504117962824,
4.06350067666592));
#13405=CARTESIAN_POINT('Ctrl Pts',(-7.52735353249786,0.663517124905538,
4.08591563261074));
#13406=CARTESIAN_POINT('Ctrl Pts',(-7.83667549320556,0.127633503183688,
4.10829588960443));
#13407=CARTESIAN_POINT('Ctrl Pts',(-7.69892862810743,-0.475216209100622,
4.13064214875721));
#13408=CARTESIAN_POINT('Ctrl Pts',(-7.24587822138796,-0.783213519985818,
4.15047591997482));
#13409=CARTESIAN_POINT('Ctrl Pts',(-6.78448909503242,-0.770150049272615,
4.16780939837816));
#13410=CARTESIAN_POINT('Ctrl Pts',(-6.44291255401028,-0.573358437418835,
4.18265244830762));
#13411=CARTESIAN_POINT('Ctrl Pts',(-6.23727444607057,-0.236582538920206,
4.19748151807985));
#13412=CARTESIAN_POINT('Ctrl Pts',(-6.21750233201011,0.156779347523281,
4.21229685032696));
#13413=CARTESIAN_POINT('Ctrl Pts',(-6.38851989967645,0.511421035774412,
4.22709868951428));
#13414=CARTESIAN_POINT('Ctrl Pts',(-6.68127276436824,0.721655369840554,
4.24065490665371));
#13415=CARTESIAN_POINT('Ctrl Pts',(-6.99873870462004,0.781500222137114,
4.25296927229394));
#13416=CARTESIAN_POINT('Ctrl Pts',(-7.28423799128053,0.727580241858167,
4.26404501085876));
#13417=CARTESIAN_POINT('Ctrl Pts',(-7.52996735384668,0.573044604556925,
4.27511366794562));
#13418=CARTESIAN_POINT('Ctrl Pts',(-7.70249233600175,0.339504000304913,
4.28617535676904));
#13419=CARTESIAN_POINT('Ctrl Pts',(-7.77704029199075,0.0596812865399207,
4.29723019232866));
#13420=CARTESIAN_POINT('Ctrl Pts',(-7.73493077249201,-0.32516426809182,
4.31196099263524));
#13421=CARTESIAN_POINT('Ctrl Pts',(-7.48195320169677,-0.642258532616097,
4.32667855077855));
#13422=CARTESIAN_POINT('Ctrl Pts',(-7.11676447072565,-0.768672906025829,
4.34138335007881));
#13423=CARTESIAN_POINT('Ctrl Pts',(-6.82822052968084,-0.75826459078673,
4.35240569057047));
#13424=CARTESIAN_POINT('Ctrl Pts',(-6.56324655367934,-0.642480501470498,
4.36342189483669));
#13425=CARTESIAN_POINT('Ctrl Pts',(-6.3590246126422,-0.438361948172784,
4.37443208856579));
#13426=CARTESIAN_POINT('Ctrl Pts',(-6.24366823031993,-0.173725992278803,
4.38543639651659));
#13427=CARTESIAN_POINT('Ctrl Pts',(-6.23278862096309,0.114603786226641,
4.39643494391794));
#13428=CARTESIAN_POINT('Ctrl Pts',(-6.32818140570146,0.3866727001158,4.40742785948479));
#13429=CARTESIAN_POINT('Ctrl Pts',(-6.54732728408833,0.641795528726263,
4.42024651101618));
#13430=CARTESIAN_POINT('Ctrl Pts',(-6.90966296029133,0.792450205988824,
4.43488744119146));
#13431=CARTESIAN_POINT('Ctrl Pts',(-7.34497884959273,0.718229352606656,
4.45134684847234));
#13432=CARTESIAN_POINT('Ctrl Pts',(-7.67373744220819,0.42439860304808,4.46779506017063));
#13433=CARTESIAN_POINT('Ctrl Pts',(-7.7957623026863,0.000795392209376382,
4.48423253597012));
#13434=CARTESIAN_POINT('Ctrl Pts',(-7.6737681501059,-0.422451523433032,
4.50065973137187));
#13435=CARTESIAN_POINT('Ctrl Pts',(-7.34550270887416,-0.715780174479536,
4.51707711746896));
#13436=CARTESIAN_POINT('Ctrl Pts',(-6.91173568096419,-0.789442989854855,
4.53348515869499));
#13437=CARTESIAN_POINT('Ctrl Pts',(-6.50548543634235,-0.62113576023861,
4.54988433137086));
#13438=CARTESIAN_POINT('Ctrl Pts',(-6.25117725190974,-0.26266942709969,
4.56627511486019));
#13439=CARTESIAN_POINT('Ctrl Pts',(-6.22657268391725,0.175941615799059,
4.58265798957595));
#13440=CARTESIAN_POINT('Ctrl Pts',(-6.43900037753832,0.560237327905976,
4.59903344336352));
#13441=CARTESIAN_POINT('Ctrl Pts',(-6.82315231070266,0.772532064615231,
4.61540196293227));
#13442=CARTESIAN_POINT('Ctrl Pts',(-7.2612181287951,0.747894614274433,4.63176404577646));
#13443=CARTESIAN_POINT('Ctrl Pts',(-7.61885424416052,0.494109349486934,
4.64812018315545));
#13444=CARTESIAN_POINT('Ctrl Pts',(-7.78669901230814,0.0889725746862699,
4.66447087596232));
#13445=CARTESIAN_POINT('Ctrl Pts',(-7.72532501848925,-0.270994143806812,
4.67809233336064));
#13446=CARTESIAN_POINT('Ctrl Pts',(-7.56738721688822,-0.506594326857297,
4.68898728035258));
#13447=CARTESIAN_POINT('Ctrl Pts',(-7.35097564028756,-0.689891456361417,
4.69988083117445));
#13448=CARTESIAN_POINT('Ctrl Pts',(-7.0003169174225,-0.79110738140522,4.71349530909451));
#13449=CARTESIAN_POINT('Ctrl Pts',(-6.57937611771461,-0.669773743535281,
4.72982925479887));
#13450=CARTESIAN_POINT('Ctrl Pts',(-6.28761734218788,-0.343284450620702,
4.74616028288309));
#13451=CARTESIAN_POINT('Ctrl Pts',(-6.21426971041073,0.0883871334668474,
4.76248890194073));
#13452=CARTESIAN_POINT('Ctrl Pts',(-6.38182100128212,0.492840639406237,
4.77881561989744));
#13453=CARTESIAN_POINT('Ctrl Pts',(-6.73884045313308,0.746153973023737,
4.79514095601288));
#13454=CARTESIAN_POINT('Ctrl Pts',(-7.17589338359863,0.770679755263529,
4.81146540426486));
#13455=CARTESIAN_POINT('Ctrl Pts',(-7.55900114520461,0.55894423669953,4.82778951061359));
#13456=CARTESIAN_POINT('Ctrl Pts',(-7.77075750409873,0.175788412965931,
4.84411370102291));
#13457=CARTESIAN_POINT('Ctrl Pts',(-7.74620736592161,-0.261233995076225,
4.86043866853608));
#13458=CARTESIAN_POINT('Ctrl Pts',(-7.49294321470503,-0.618448872812403,
4.87676449790797));
#13459=CARTESIAN_POINT('Ctrl Pts',(-7.08837163954946,-0.785730122461179,
4.89309260172666));
#13460=CARTESIAN_POINT('Ctrl Pts',(-6.65674407499508,-0.712671607108413,
4.90942182102584));
#13461=CARTESIAN_POINT('Ctrl Pts',(-6.33017289353631,-0.420518596063947,
4.92575590410514));
#13462=CARTESIAN_POINT('Ctrl Pts',(-6.2493887150478,-0.140566474730618,
4.93664355063335));
#13463=CARTESIAN_POINT('Ctrl Pts',(-6.24936976727053,0.000312488344807942,
4.94209250793942));
#13464=CARTESIAN_POINT('Origin',(-6.2,-3.91353616180368E-15,4.95));
#13465=CARTESIAN_POINT('Origin',(-6.2,-3.91353616180368E-15,4.95));
#13466=CARTESIAN_POINT('Origin',(-6.2,-1.64817900953001E-18,1.05));
#13467=CARTESIAN_POINT('',(0.,0.,0.));
#13468=CARTESIAN_POINT('Origin',(3.,-2.6,6.));
#13469=CARTESIAN_POINT('',(3.46969377779353,-1.8,6.17142857142857));
#13470=CARTESIAN_POINT('',(2.53030622220647,-1.8,6.17142857142857));
#13471=CARTESIAN_POINT('Origin',(3.,-1.875,6.));
#13472=CARTESIAN_POINT('Origin',(3.,-1.8,6.));
#13473=CARTESIAN_POINT('Origin',(3.,-1.8,6.));
#13474=CARTESIAN_POINT('',(3.21502847462129,-1.8,6.17142857142857));
#13475=CARTESIAN_POINT('',(2.7,-1.8,6.17142857142857));
#13476=CARTESIAN_POINT('',(2.725,-1.8,6.));
#13477=CARTESIAN_POINT('Origin',(3.,-1.8,6.));
#13478=CARTESIAN_POINT('',(2.78497152537871,-1.8,6.17142857142857));
#13479=CARTESIAN_POINT('Origin',(3.,-1.8,6.));
#13480=CARTESIAN_POINT('',(2.7,-1.8,6.17142857142857));
#13481=CARTESIAN_POINT('Origin',(2.4,-1.,8.));
#13482=CARTESIAN_POINT('',(2.4,-4.5,0.));
#13483=CARTESIAN_POINT('',(2.4,-1.,8.));
#13484=CARTESIAN_POINT('',(2.4,-4.5,0.));
#13485=CARTESIAN_POINT('',(3.6,-4.5,0.));
#13486=CARTESIAN_POINT('',(2.4,-4.5,0.));
#13487=CARTESIAN_POINT('',(3.6,-1.,8.));
#13488=CARTESIAN_POINT('',(3.6,-4.5,0.));
#13489=CARTESIAN_POINT('',(2.4,-1.,8.));
#13490=CARTESIAN_POINT('',(2.84387505004004,-3.975,1.2));
#13491=CARTESIAN_POINT('',(3.15612494995996,-3.975,1.2));
#13492=CARTESIAN_POINT('Origin',(3.,-3.5,2.28571428571429));
#13493=CARTESIAN_POINT('',(2.7,-3.975,1.2));
#13494=CARTESIAN_POINT('Origin',(3.,-1.875,6.));
#13495=CARTESIAN_POINT('Origin',(3.,-2.6,6.));
#13496=CARTESIAN_POINT('',(2.725,-1.,6.));
#13497=CARTESIAN_POINT('',(2.725,-2.6,6.));
#13498=CARTESIAN_POINT('Origin',(3.,-1.,6.));
#13499=CARTESIAN_POINT('Origin',(3.,-3.5,1.2));
#13500=CARTESIAN_POINT('Origin',(3.,-3.5,1.2));
#13501=CARTESIAN_POINT('',(2.725,-3.5,1.2));
#13502=CARTESIAN_POINT('Origin',(3.,-3.5,1.2));
#13503=CARTESIAN_POINT('Origin',(3.,-3.5,1.2));
#13504=CARTESIAN_POINT('Origin',(3.,-3.5,-0.1));
#13505=CARTESIAN_POINT('',(2.725,-3.5,0.));
#13506=CARTESIAN_POINT('Origin',(3.,-3.5,0.));
#13507=CARTESIAN_POINT('',(2.725,-3.5,-0.1));
#13508=CARTESIAN_POINT('Origin',(2.4,-1.,0.));
#13509=CARTESIAN_POINT('',(2.4,-1.,0.));
#13510=CARTESIAN_POINT('',(2.4,-1.,8.));
#13511=CARTESIAN_POINT('',(3.6,-1.,0.));
#13512=CARTESIAN_POINT('',(3.6,-1.,8.));
#13513=CARTESIAN_POINT('',(2.4,-1.,0.));
#13514=CARTESIAN_POINT('Origin',(2.4,-4.5,0.));
#13515=CARTESIAN_POINT('',(2.4,-1.,0.));
#13516=CARTESIAN_POINT('',(3.6,-1.,0.));
#13517=CARTESIAN_POINT('Origin',(3.6,-2.75,4.));
#13518=CARTESIAN_POINT('Origin',(2.4,-2.75,4.));
#13519=CARTESIAN_POINT('',(0.,0.,0.));
#13520=CARTESIAN_POINT('Origin',(3.,1.8,6.));
#13521=CARTESIAN_POINT('',(2.53030622220647,1.8,6.17142857142857));
#13522=CARTESIAN_POINT('',(3.46969377779353,1.8,6.17142857142857));
#13523=CARTESIAN_POINT('Origin',(3.,1.875,6.));
#13524=CARTESIAN_POINT('Origin',(3.,1.8,6.));
#13525=CARTESIAN_POINT('Origin',(3.,1.8,6.));
#13526=CARTESIAN_POINT('',(2.78497152537871,1.8,6.17142857142857));
#13527=CARTESIAN_POINT('',(2.7,1.8,6.17142857142857));
#13528=CARTESIAN_POINT('',(2.725,1.8,6.));
#13529=CARTESIAN_POINT('Origin',(3.,1.8,6.));
#13530=CARTESIAN_POINT('',(3.21502847462129,1.8,6.17142857142857));
#13531=CARTESIAN_POINT('Origin',(3.,1.8,6.));
#13532=CARTESIAN_POINT('',(2.7,1.8,6.17142857142857));
#13533=CARTESIAN_POINT('Origin',(2.4,4.5,0.));
#13534=CARTESIAN_POINT('',(2.4,4.5,0.));
#13535=CARTESIAN_POINT('',(2.4,1.,8.));
#13536=CARTESIAN_POINT('',(2.4,4.5,0.));
#13537=CARTESIAN_POINT('',(3.6,1.,8.));
#13538=CARTESIAN_POINT('',(2.4,1.,8.));
#13539=CARTESIAN_POINT('',(3.6,4.5,0.));
#13540=CARTESIAN_POINT('',(3.6,4.5,0.));
#13541=CARTESIAN_POINT('',(2.4,4.5,0.));
#13542=CARTESIAN_POINT('',(3.15612494995996,3.975,1.2));
#13543=CARTESIAN_POINT('',(2.84387505004004,3.975,1.2));
#13544=CARTESIAN_POINT('Origin',(3.,3.5,2.28571428571429));
#13545=CARTESIAN_POINT('',(2.7,3.975,1.2));
#13546=CARTESIAN_POINT('Origin',(3.,1.875,6.));
#13547=CARTESIAN_POINT('Origin',(3.,0.9,6.));
#13548=CARTESIAN_POINT('',(2.725,1.,6.));
#13549=CARTESIAN_POINT('Origin',(3.,1.,6.));
#13550=CARTESIAN_POINT('',(2.725,0.9,6.));
#13551=CARTESIAN_POINT('Origin',(3.,3.5,1.2));
#13552=CARTESIAN_POINT('Origin',(3.,3.5,1.2));
#13553=CARTESIAN_POINT('',(2.725,3.5,1.2));
#13554=CARTESIAN_POINT('Origin',(3.,3.5,1.2));
#13555=CARTESIAN_POINT('Origin',(3.,3.5,1.2));
#13556=CARTESIAN_POINT('Origin',(3.,3.5,-0.1));
#13557=CARTESIAN_POINT('',(2.725,3.5,0.));
#13558=CARTESIAN_POINT('Origin',(3.,3.5,0.));
#13559=CARTESIAN_POINT('',(2.725,3.5,-0.1));
#13560=CARTESIAN_POINT('Origin',(2.4,1.,0.));
#13561=CARTESIAN_POINT('',(2.4,1.,0.));
#13562=CARTESIAN_POINT('',(2.4,1.,0.));
#13563=CARTESIAN_POINT('',(3.6,1.,0.));
#13564=CARTESIAN_POINT('',(3.6,1.,0.));
#13565=CARTESIAN_POINT('',(2.4,1.,0.));
#13566=CARTESIAN_POINT('Origin',(2.4,1.,8.));
#13567=CARTESIAN_POINT('',(2.4,1.,8.));
#13568=CARTESIAN_POINT('',(3.6,1.,8.));
#13569=CARTESIAN_POINT('Origin',(3.6,2.75,4.));
#13570=CARTESIAN_POINT('Origin',(2.4,2.75,4.));
#13571=CARTESIAN_POINT('',(0.,0.,0.));
#13572=CARTESIAN_POINT('Origin',(-0.1,0.82,-0.3));
#13573=CARTESIAN_POINT('',(0.,0.82,-0.3));
#13574=CARTESIAN_POINT('',(0.,1.,-0.3));
#13575=CARTESIAN_POINT('',(0.,0.41,-0.3));
#13576=CARTESIAN_POINT('',(40.,0.82,-0.3));
#13577=CARTESIAN_POINT('',(-0.1,0.82,-0.3));
#13578=CARTESIAN_POINT('',(40.,1.,-0.3));
#13579=CARTESIAN_POINT('',(40.,0.41,-0.3));
#13580=CARTESIAN_POINT('',(-0.05,1.,-0.3));
#13581=CARTESIAN_POINT('Origin',(-0.1,0.82,-0.55));
#13582=CARTESIAN_POINT('',(0.,0.82,-0.55));
#13583=CARTESIAN_POINT('',(0.,0.82,-0.275));
#13584=CARTESIAN_POINT('',(40.,0.82,-0.55));
#13585=CARTESIAN_POINT('',(-0.1,0.82,-0.55));
#13586=CARTESIAN_POINT('',(40.,0.82,-0.275));
#13587=CARTESIAN_POINT('Origin',(-0.1,0.67,-0.55));
#13588=CARTESIAN_POINT('',(0.,0.67,-0.55));
#13589=CARTESIAN_POINT('',(0.,0.335,-0.55));
#13590=CARTESIAN_POINT('',(40.,0.67,-0.55));
#13591=CARTESIAN_POINT('',(-0.1,0.67,-0.55));
#13592=CARTESIAN_POINT('',(40.,0.335,-0.55));
#13593=CARTESIAN_POINT('Origin',(-0.1,0.42,-0.3));
#13594=CARTESIAN_POINT('',(0.,0.42,-0.3));
#13595=CARTESIAN_POINT('',(0.,0.24,-0.12));
#13596=CARTESIAN_POINT('',(40.,0.42,-0.3));
#13597=CARTESIAN_POINT('',(-0.1,0.42,-0.3));
#13598=CARTESIAN_POINT('',(40.,0.24,-0.12));
#13599=CARTESIAN_POINT('Origin',(-0.1,0.42,0.3));
#13600=CARTESIAN_POINT('',(0.,0.42,0.3));
#13601=CARTESIAN_POINT('',(0.,0.42,0.15));
#13602=CARTESIAN_POINT('',(40.,0.42,0.3));
#13603=CARTESIAN_POINT('',(-0.1,0.42,0.3));
#13604=CARTESIAN_POINT('',(40.,0.42,0.15));
#13605=CARTESIAN_POINT('Origin',(-0.1,0.67,0.55));
#13606=CARTESIAN_POINT('',(0.,0.67,0.55));
#13607=CARTESIAN_POINT('',(6.93889390390723E-18,0.365,0.245));
#13608=CARTESIAN_POINT('',(40.,0.67,0.55));
#13609=CARTESIAN_POINT('',(-0.1,0.67,0.55));
#13610=CARTESIAN_POINT('',(40.,0.365,0.245));
#13611=CARTESIAN_POINT('Origin',(-0.1,0.82,0.55));
#13612=CARTESIAN_POINT('',(0.,0.82,0.55));
#13613=CARTESIAN_POINT('',(0.,0.41,0.55));
#13614=CARTESIAN_POINT('',(40.,0.82,0.55));
#13615=CARTESIAN_POINT('',(-0.1,0.82,0.55));
#13616=CARTESIAN_POINT('',(40.,0.41,0.55));
#13617=CARTESIAN_POINT('Origin',(-0.1,0.82,0.3));
#13618=CARTESIAN_POINT('',(0.,0.82,0.3));
#13619=CARTESIAN_POINT('',(0.,0.82,0.15));
#13620=CARTESIAN_POINT('',(40.,0.82,0.3));
#13621=CARTESIAN_POINT('',(-0.1,0.82,0.3));
#13622=CARTESIAN_POINT('',(40.,0.82,0.15));
#13623=CARTESIAN_POINT('Origin',(-0.1,1.05,0.3));
#13624=CARTESIAN_POINT('',(0.,1.,0.3));
#13625=CARTESIAN_POINT('',(0.,0.525,0.3));
#13626=CARTESIAN_POINT('',(40.,1.,0.3));
#13627=CARTESIAN_POINT('',(-0.05,1.,0.3));
#13628=CARTESIAN_POINT('',(40.,0.525,0.3));
#13629=CARTESIAN_POINT('Origin',(-0.1,-0.3,-0.82));
#13630=CARTESIAN_POINT('',(0.,-0.3,-0.82));
#13631=CARTESIAN_POINT('',(0.,-0.3,-1.));
#13632=CARTESIAN_POINT('',(0.,-0.3,-0.41));
#13633=CARTESIAN_POINT('',(40.,-0.3,-0.82));
#13634=CARTESIAN_POINT('',(-0.1,-0.3,-0.82));
#13635=CARTESIAN_POINT('',(40.,-0.3,-1.));
#13636=CARTESIAN_POINT('',(40.,-0.3,-0.41));
#13637=CARTESIAN_POINT('',(-0.05,-0.3,-1.));
#13638=CARTESIAN_POINT('Origin',(-0.1,-0.55,-0.82));
#13639=CARTESIAN_POINT('',(0.,-0.55,-0.82));
#13640=CARTESIAN_POINT('',(0.,-0.275,-0.82));
#13641=CARTESIAN_POINT('',(40.,-0.55,-0.82));
#13642=CARTESIAN_POINT('',(-0.1,-0.55,-0.82));
#13643=CARTESIAN_POINT('',(40.,-0.275,-0.82));
#13644=CARTESIAN_POINT('Origin',(-0.1,-0.55,-0.67));
#13645=CARTESIAN_POINT('',(0.,-0.55,-0.67));
#13646=CARTESIAN_POINT('',(0.,-0.55,-0.335));
#13647=CARTESIAN_POINT('',(40.,-0.55,-0.67));
#13648=CARTESIAN_POINT('',(-0.1,-0.55,-0.67));
#13649=CARTESIAN_POINT('',(40.,-0.55,-0.335));
#13650=CARTESIAN_POINT('Origin',(-0.1,-0.3,-0.42));
#13651=CARTESIAN_POINT('',(0.,-0.3,-0.42));
#13652=CARTESIAN_POINT('',(0.,-0.12,-0.24));
#13653=CARTESIAN_POINT('',(40.,-0.3,-0.42));
#13654=CARTESIAN_POINT('',(-0.1,-0.3,-0.42));
#13655=CARTESIAN_POINT('',(40.,-0.12,-0.24));
#13656=CARTESIAN_POINT('Origin',(-0.1,0.3,-0.42));
#13657=CARTESIAN_POINT('',(0.,0.3,-0.42));
#13658=CARTESIAN_POINT('',(0.,0.15,-0.42));
#13659=CARTESIAN_POINT('',(40.,0.3,-0.42));
#13660=CARTESIAN_POINT('',(-0.1,0.3,-0.42));
#13661=CARTESIAN_POINT('',(40.,0.15,-0.42));
#13662=CARTESIAN_POINT('Origin',(-0.1,0.55,-0.67));
#13663=CARTESIAN_POINT('',(0.,0.55,-0.67));
#13664=CARTESIAN_POINT('',(0.,0.245,-0.365));
#13665=CARTESIAN_POINT('',(40.,0.55,-0.67));
#13666=CARTESIAN_POINT('',(-0.1,0.55,-0.67));
#13667=CARTESIAN_POINT('',(40.,0.245,-0.365));
#13668=CARTESIAN_POINT('Origin',(-0.1,0.55,-0.82));
#13669=CARTESIAN_POINT('',(0.,0.55,-0.82));
#13670=CARTESIAN_POINT('',(0.,0.55,-0.41));
#13671=CARTESIAN_POINT('',(40.,0.55,-0.82));
#13672=CARTESIAN_POINT('',(-0.1,0.55,-0.82));
#13673=CARTESIAN_POINT('',(40.,0.55,-0.41));
#13674=CARTESIAN_POINT('Origin',(-0.1,0.3,-0.82));
#13675=CARTESIAN_POINT('',(0.,0.3,-0.82));
#13676=CARTESIAN_POINT('',(0.,0.15,-0.82));
#13677=CARTESIAN_POINT('',(40.,0.3,-0.82));
#13678=CARTESIAN_POINT('',(-0.1,0.3,-0.82));
#13679=CARTESIAN_POINT('',(40.,0.15,-0.82));
#13680=CARTESIAN_POINT('Origin',(-0.1,0.3,-1.05));
#13681=CARTESIAN_POINT('',(0.,0.3,-1.));
#13682=CARTESIAN_POINT('',(0.,0.3,-0.525));
#13683=CARTESIAN_POINT('',(40.,0.3,-1.));
#13684=CARTESIAN_POINT('',(-0.05,0.3,-1.));
#13685=CARTESIAN_POINT('',(40.,0.3,-0.525));
#13686=CARTESIAN_POINT('Origin',(-0.1,-0.82,0.3));
#13687=CARTESIAN_POINT('',(0.,-0.82,0.3));
#13688=CARTESIAN_POINT('',(0.,-1.,0.3));
#13689=CARTESIAN_POINT('',(0.,-0.41,0.3));
#13690=CARTESIAN_POINT('',(40.,-0.82,0.3));
#13691=CARTESIAN_POINT('',(-0.1,-0.82,0.3));
#13692=CARTESIAN_POINT('',(40.,-1.,0.3));
#13693=CARTESIAN_POINT('',(40.,-0.41,0.3));
#13694=CARTESIAN_POINT('',(-0.05,-1.,0.3));
#13695=CARTESIAN_POINT('Origin',(-0.1,-0.82,0.55));
#13696=CARTESIAN_POINT('',(0.,-0.82,0.55));
#13697=CARTESIAN_POINT('',(0.,-0.82,0.275));
#13698=CARTESIAN_POINT('',(40.,-0.82,0.55));
#13699=CARTESIAN_POINT('',(-0.1,-0.82,0.55));
#13700=CARTESIAN_POINT('',(40.,-0.82,0.275));
#13701=CARTESIAN_POINT('Origin',(-0.1,-0.67,0.55));
#13702=CARTESIAN_POINT('',(0.,-0.67,0.55));
#13703=CARTESIAN_POINT('',(0.,-0.335,0.55));
#13704=CARTESIAN_POINT('',(40.,-0.67,0.55));
#13705=CARTESIAN_POINT('',(-0.1,-0.67,0.55));
#13706=CARTESIAN_POINT('',(40.,-0.335,0.55));
#13707=CARTESIAN_POINT('Origin',(-0.1,-0.42,0.3));
#13708=CARTESIAN_POINT('',(0.,-0.42,0.3));
#13709=CARTESIAN_POINT('',(-6.93889390390723E-18,-0.24,0.12));
#13710=CARTESIAN_POINT('',(40.,-0.42,0.3));
#13711=CARTESIAN_POINT('',(-0.1,-0.42,0.3));
#13712=CARTESIAN_POINT('',(40.,-0.24,0.12));
#13713=CARTESIAN_POINT('Origin',(-0.1,-0.42,-0.3));
#13714=CARTESIAN_POINT('',(0.,-0.42,-0.3));
#13715=CARTESIAN_POINT('',(0.,-0.42,-0.15));
#13716=CARTESIAN_POINT('',(40.,-0.42,-0.3));
#13717=CARTESIAN_POINT('',(-0.1,-0.42,-0.3));
#13718=CARTESIAN_POINT('',(40.,-0.42,-0.15));
#13719=CARTESIAN_POINT('Origin',(-0.1,-0.67,-0.55));
#13720=CARTESIAN_POINT('',(0.,-0.67,-0.55));
#13721=CARTESIAN_POINT('',(0.,-0.365,-0.245));
#13722=CARTESIAN_POINT('',(40.,-0.67,-0.55));
#13723=CARTESIAN_POINT('',(-0.1,-0.67,-0.55));
#13724=CARTESIAN_POINT('',(40.,-0.365,-0.245));
#13725=CARTESIAN_POINT('Origin',(-0.1,-0.82,-0.55));
#13726=CARTESIAN_POINT('',(0.,-0.82,-0.55));
#13727=CARTESIAN_POINT('',(0.,-0.41,-0.55));
#13728=CARTESIAN_POINT('',(40.,-0.82,-0.55));
#13729=CARTESIAN_POINT('',(-0.1,-0.82,-0.55));
#13730=CARTESIAN_POINT('',(40.,-0.41,-0.55));
#13731=CARTESIAN_POINT('Origin',(-0.1,-0.82,-0.3));
#13732=CARTESIAN_POINT('',(0.,-0.82,-0.3));
#13733=CARTESIAN_POINT('',(0.,-0.82,-0.15));
#13734=CARTESIAN_POINT('',(40.,-0.82,-0.3));
#13735=CARTESIAN_POINT('',(-0.1,-0.82,-0.3));
#13736=CARTESIAN_POINT('',(40.,-0.82,-0.15));
#13737=CARTESIAN_POINT('Origin',(-0.1,-1.05,-0.3));
#13738=CARTESIAN_POINT('',(0.,-1.,-0.3));
#13739=CARTESIAN_POINT('',(0.,-0.525,-0.3));
#13740=CARTESIAN_POINT('',(40.,-1.,-0.3));
#13741=CARTESIAN_POINT('',(-0.05,-1.,-0.3));
#13742=CARTESIAN_POINT('',(40.,-0.525,-0.3));
#13743=CARTESIAN_POINT('Origin',(-0.1,0.3,0.82));
#13744=CARTESIAN_POINT('',(0.,0.3,0.82));
#13745=CARTESIAN_POINT('',(0.,0.3,1.));
#13746=CARTESIAN_POINT('',(0.,0.3,0.41));
#13747=CARTESIAN_POINT('',(40.,0.3,0.82));
#13748=CARTESIAN_POINT('',(-0.1,0.3,0.82));
#13749=CARTESIAN_POINT('',(40.,0.3,1.));
#13750=CARTESIAN_POINT('',(40.,0.3,0.41));
#13751=CARTESIAN_POINT('',(-0.05,0.3,1.));
#13752=CARTESIAN_POINT('Origin',(-0.1,0.55,0.82));
#13753=CARTESIAN_POINT('',(0.,0.55,0.82));
#13754=CARTESIAN_POINT('',(0.,0.275,0.82));
#13755=CARTESIAN_POINT('',(40.,0.55,0.82));
#13756=CARTESIAN_POINT('',(-0.1,0.55,0.82));
#13757=CARTESIAN_POINT('',(40.,0.275,0.82));
#13758=CARTESIAN_POINT('Origin',(-0.1,0.55,0.67));
#13759=CARTESIAN_POINT('',(0.,0.55,0.67));
#13760=CARTESIAN_POINT('',(0.,0.55,0.335));
#13761=CARTESIAN_POINT('',(40.,0.55,0.67));
#13762=CARTESIAN_POINT('',(-0.1,0.55,0.67));
#13763=CARTESIAN_POINT('',(40.,0.55,0.335));
#13764=CARTESIAN_POINT('Origin',(-0.1,0.3,0.42));
#13765=CARTESIAN_POINT('',(0.,0.3,0.42));
#13766=CARTESIAN_POINT('',(6.93889390390723E-18,0.12,0.24));
#13767=CARTESIAN_POINT('',(40.,0.3,0.42));
#13768=CARTESIAN_POINT('',(-0.1,0.3,0.42));
#13769=CARTESIAN_POINT('',(40.,0.12,0.24));
#13770=CARTESIAN_POINT('Origin',(-0.1,-0.3,0.42));
#13771=CARTESIAN_POINT('',(0.,-0.3,0.42));
#13772=CARTESIAN_POINT('',(0.,-0.15,0.42));
#13773=CARTESIAN_POINT('',(40.,-0.3,0.42));
#13774=CARTESIAN_POINT('',(-0.1,-0.3,0.42));
#13775=CARTESIAN_POINT('',(40.,-0.15,0.42));
#13776=CARTESIAN_POINT('Origin',(-0.1,-0.55,0.67));
#13777=CARTESIAN_POINT('',(0.,-0.55,0.67));
#13778=CARTESIAN_POINT('',(6.93889390390723E-18,-0.245,0.365));
#13779=CARTESIAN_POINT('',(40.,-0.55,0.67));
#13780=CARTESIAN_POINT('',(-0.1,-0.55,0.67));
#13781=CARTESIAN_POINT('',(40.,-0.245,0.365));
#13782=CARTESIAN_POINT('Origin',(-0.1,-0.55,0.82));
#13783=CARTESIAN_POINT('',(0.,-0.55,0.82));
#13784=CARTESIAN_POINT('',(0.,-0.55,0.41));
#13785=CARTESIAN_POINT('',(40.,-0.55,0.82));
#13786=CARTESIAN_POINT('',(-0.1,-0.55,0.82));
#13787=CARTESIAN_POINT('',(40.,-0.55,0.41));
#13788=CARTESIAN_POINT('Origin',(-0.1,-0.3,0.82));
#13789=CARTESIAN_POINT('',(0.,-0.3,0.82));
#13790=CARTESIAN_POINT('',(0.,-0.15,0.82));
#13791=CARTESIAN_POINT('',(40.,-0.3,0.82));
#13792=CARTESIAN_POINT('',(-0.1,-0.3,0.82));
#13793=CARTESIAN_POINT('',(40.,-0.15,0.82));
#13794=CARTESIAN_POINT('Origin',(-0.1,-0.3,1.05));
#13795=CARTESIAN_POINT('',(0.,-0.3,1.));
#13796=CARTESIAN_POINT('',(0.,-0.3,0.525));
#13797=CARTESIAN_POINT('',(40.,-0.3,1.));
#13798=CARTESIAN_POINT('',(-0.05,-0.3,1.));
#13799=CARTESIAN_POINT('',(40.,-0.3,0.525));
#13800=CARTESIAN_POINT('Origin',(-0.1,0.,0.));
#13801=CARTESIAN_POINT('',(0.,-2.57175827820944E-17,0.21));
#13802=CARTESIAN_POINT('Origin',(0.,0.,0.));
#13803=CARTESIAN_POINT('',(40.,2.57175827820944E-17,0.21));
#13804=CARTESIAN_POINT('',(-0.1,-2.57175827820944E-17,0.21));
#13805=CARTESIAN_POINT('Origin',(40.,0.,0.));
#13806=CARTESIAN_POINT('Origin',(0.,1.,-1.));
#13807=CARTESIAN_POINT('',(0.,1.,1.));
#13808=CARTESIAN_POINT('',(0.,1.,-1.));
#13809=CARTESIAN_POINT('',(40.,1.,1.));
#13810=CARTESIAN_POINT('',(0.,1.,1.));
#13811=CARTESIAN_POINT('',(40.,1.,-1.));
#13812=CARTESIAN_POINT('Origin',(0.,1.,-1.));
#13813=CARTESIAN_POINT('',(40.,1.,-1.));
#13814=CARTESIAN_POINT('',(40.,1.,-1.));
#13815=CARTESIAN_POINT('',(0.,1.,-1.));
#13816=CARTESIAN_POINT('',(0.,1.,-1.));
#13817=CARTESIAN_POINT('',(0.,1.,-1.));
#13818=CARTESIAN_POINT('Origin',(0.,-1.,-1.));
#13819=CARTESIAN_POINT('',(0.,-1.,-1.));
#13820=CARTESIAN_POINT('',(40.,-1.,-1.));
#13821=CARTESIAN_POINT('Origin',(0.,-1.,-1.));
#13822=CARTESIAN_POINT('',(40.,-1.,-1.));
#13823=CARTESIAN_POINT('',(40.,-1.,-1.));
#13824=CARTESIAN_POINT('',(0.,-1.,-1.));
#13825=CARTESIAN_POINT('',(0.,-1.,-1.));
#13826=CARTESIAN_POINT('',(0.,-1.,-1.));
#13827=CARTESIAN_POINT('Origin',(0.,-1.,1.));
#13828=CARTESIAN_POINT('',(0.,-1.,1.));
#13829=CARTESIAN_POINT('',(40.,-1.,1.));
#13830=CARTESIAN_POINT('Origin',(0.,-1.,1.));
#13831=CARTESIAN_POINT('',(40.,-1.,1.));
#13832=CARTESIAN_POINT('',(40.,-1.,1.));
#13833=CARTESIAN_POINT('',(0.,-1.,1.));
#13834=CARTESIAN_POINT('',(0.,-1.,1.));
#13835=CARTESIAN_POINT('',(0.,-1.,1.));
#13836=CARTESIAN_POINT('Origin',(0.,1.,1.));
#13837=CARTESIAN_POINT('',(0.,1.,1.));
#13838=CARTESIAN_POINT('',(40.,1.,1.));
#13839=CARTESIAN_POINT('Origin',(0.,1.,1.));
#13840=CARTESIAN_POINT('',(40.,1.,1.));
#13841=CARTESIAN_POINT('',(0.,1.,1.));
#13842=CARTESIAN_POINT('Origin',(40.,0.,0.));
#13843=CARTESIAN_POINT('Origin',(0.,0.,0.));
#13844=CARTESIAN_POINT('',(0.,0.,0.));
#13845=CARTESIAN_POINT('Origin',(14.,0.,0.97));
#13846=CARTESIAN_POINT('',(13.625,-4.59242549680257E-17,0.97));
#13847=CARTESIAN_POINT('Origin',(14.,0.,0.97));
#13848=CARTESIAN_POINT('',(13.625,4.59242549680257E-17,1.5));
#13849=CARTESIAN_POINT('',(13.625,-4.59242549680257E-17,0.97));
#13850=CARTESIAN_POINT('Origin',(14.,0.,1.5));
#13851=CARTESIAN_POINT('Origin',(14.,0.,0.97));
#13852=CARTESIAN_POINT('',(13.775,-2.75545529808154E-17,0.97));
#13853=CARTESIAN_POINT('Origin',(14.,0.,0.97));
#13854=CARTESIAN_POINT('Origin',(8.,0.,0.97));
#13855=CARTESIAN_POINT('',(7.625,-4.59242549680257E-17,0.97));
#13856=CARTESIAN_POINT('Origin',(8.,0.,0.97));
#13857=CARTESIAN_POINT('',(7.625,4.59242549680257E-17,1.5));
#13858=CARTESIAN_POINT('',(7.625,-4.59242549680257E-17,0.97));
#13859=CARTESIAN_POINT('Origin',(8.,0.,1.5));
#13860=CARTESIAN_POINT('Origin',(8.,0.,0.97));
#13861=CARTESIAN_POINT('',(7.775,-2.75545529808154E-17,0.97));
#13862=CARTESIAN_POINT('Origin',(8.,0.,0.97));
#13863=CARTESIAN_POINT('Origin',(2.,0.,0.97));
#13864=CARTESIAN_POINT('',(1.625,-4.59242549680257E-17,0.97));
#13865=CARTESIAN_POINT('Origin',(2.,0.,0.97));
#13866=CARTESIAN_POINT('',(1.625,4.59242549680257E-17,1.5));
#13867=CARTESIAN_POINT('',(1.625,-4.59242549680257E-17,0.97));
#13868=CARTESIAN_POINT('Origin',(2.,0.,1.5));
#13869=CARTESIAN_POINT('Origin',(2.,0.,0.97));
#13870=CARTESIAN_POINT('',(1.775,-2.75545529808155E-17,0.97));
#13871=CARTESIAN_POINT('Origin',(2.,0.,0.97));
#13872=CARTESIAN_POINT('Origin',(20.,0.,0.97));
#13873=CARTESIAN_POINT('',(19.625,-4.59242549680257E-17,0.97));
#13874=CARTESIAN_POINT('Origin',(20.,0.,0.97));
#13875=CARTESIAN_POINT('',(19.625,4.59242549680257E-17,1.5));
#13876=CARTESIAN_POINT('',(19.625,-4.59242549680257E-17,0.97));
#13877=CARTESIAN_POINT('Origin',(20.,0.,1.5));
#13878=CARTESIAN_POINT('Origin',(20.,0.,0.97));
#13879=CARTESIAN_POINT('',(19.775,-2.75545529808156E-17,0.97));
#13880=CARTESIAN_POINT('Origin',(20.,0.,0.97));
#13881=CARTESIAN_POINT('Origin',(14.,0.,-0.1));
#13882=CARTESIAN_POINT('',(13.775,-2.75545529808154E-17,0.));
#13883=CARTESIAN_POINT('Origin',(14.,0.,0.));
#13884=CARTESIAN_POINT('',(13.775,-2.75545529808154E-17,-0.1));
#13885=CARTESIAN_POINT('Origin',(8.,0.,-0.1));
#13886=CARTESIAN_POINT('',(7.775,-2.75545529808154E-17,0.));
#13887=CARTESIAN_POINT('Origin',(8.,0.,0.));
#13888=CARTESIAN_POINT('',(7.775,-2.75545529808154E-17,-0.1));
#13889=CARTESIAN_POINT('Origin',(2.,0.,-0.1));
#13890=CARTESIAN_POINT('',(1.775,-2.75545529808155E-17,0.));
#13891=CARTESIAN_POINT('Origin',(2.,0.,0.));
#13892=CARTESIAN_POINT('',(1.775,-2.75545529808155E-17,-0.1));
#13893=CARTESIAN_POINT('Origin',(20.,0.,-0.1));
#13894=CARTESIAN_POINT('',(19.775,-2.75545529808156E-17,0.));
#13895=CARTESIAN_POINT('Origin',(20.,0.,0.));
#13896=CARTESIAN_POINT('',(19.775,-2.75545529808156E-17,-0.1));
#13897=CARTESIAN_POINT('Origin',(0.,-0.53,1.));
#13898=CARTESIAN_POINT('',(0.,-0.53,1.));
#13899=CARTESIAN_POINT('',(0.,-0.75,0.85));
#13900=CARTESIAN_POINT('',(0.,-0.53,1.));
#13901=CARTESIAN_POINT('',(22.,-0.75,0.85));
#13902=CARTESIAN_POINT('',(0.,-0.75,0.85));
#13903=CARTESIAN_POINT('',(22.,-0.53,1.));
#13904=CARTESIAN_POINT('',(22.,-0.53,1.));
#13905=CARTESIAN_POINT('',(0.,-0.53,1.));
#13906=CARTESIAN_POINT('Origin',(0.,-0.53,1.15));
#13907=CARTESIAN_POINT('',(0.,-0.53,1.15));
#13908=CARTESIAN_POINT('',(0.,-0.53,1.15));
#13909=CARTESIAN_POINT('',(22.,-0.53,1.15));
#13910=CARTESIAN_POINT('',(22.,-0.53,1.15));
#13911=CARTESIAN_POINT('',(0.,-0.53,1.15));
#13912=CARTESIAN_POINT('Origin',(0.,-0.75,1.3));
#13913=CARTESIAN_POINT('',(0.,-0.75,1.3));
#13914=CARTESIAN_POINT('',(0.,-0.75,1.3));
#13915=CARTESIAN_POINT('',(22.,-0.75,1.3));
#13916=CARTESIAN_POINT('',(22.,-0.75,1.3));
#13917=CARTESIAN_POINT('',(0.,-0.75,1.3));
#13918=CARTESIAN_POINT('Origin',(0.,-0.75,1.5));
#13919=CARTESIAN_POINT('',(0.,-0.75,1.5));
#13920=CARTESIAN_POINT('',(0.,-0.75,1.5));
#13921=CARTESIAN_POINT('',(22.,-0.75,1.5));
#13922=CARTESIAN_POINT('',(22.,-0.75,1.5));
#13923=CARTESIAN_POINT('',(0.,-0.75,1.5));
#13924=CARTESIAN_POINT('Origin',(0.,0.75,1.5));
#13925=CARTESIAN_POINT('',(0.,0.75,1.5));
#13926=CARTESIAN_POINT('',(0.,0.75,1.5));
#13927=CARTESIAN_POINT('',(22.,0.75,1.5));
#13928=CARTESIAN_POINT('',(22.,0.75,1.5));
#13929=CARTESIAN_POINT('',(0.,0.75,1.5));
#13930=CARTESIAN_POINT('Origin',(0.,0.75,1.3));
#13931=CARTESIAN_POINT('',(0.,0.75,1.3));
#13932=CARTESIAN_POINT('',(0.,0.75,1.3));
#13933=CARTESIAN_POINT('',(22.,0.75,1.3));
#13934=CARTESIAN_POINT('',(22.,0.75,1.3));
#13935=CARTESIAN_POINT('',(0.,0.75,1.3));
#13936=CARTESIAN_POINT('Origin',(0.,0.53,1.15));
#13937=CARTESIAN_POINT('',(0.,0.53,1.15));
#13938=CARTESIAN_POINT('',(0.,0.53,1.15));
#13939=CARTESIAN_POINT('',(22.,0.53,1.15));
#13940=CARTESIAN_POINT('',(22.,0.53,1.15));
#13941=CARTESIAN_POINT('',(0.,0.53,1.15));
#13942=CARTESIAN_POINT('Origin',(0.,0.53,1.));
#13943=CARTESIAN_POINT('',(0.,0.53,1.));
#13944=CARTESIAN_POINT('',(0.,0.53,1.));
#13945=CARTESIAN_POINT('',(22.,0.53,1.));
#13946=CARTESIAN_POINT('',(22.,0.53,1.));
#13947=CARTESIAN_POINT('',(0.,0.53,1.));
#13948=CARTESIAN_POINT('Origin',(0.,0.75,0.85));
#13949=CARTESIAN_POINT('',(0.,0.75,0.85));
#13950=CARTESIAN_POINT('',(0.,0.75,0.85));
#13951=CARTESIAN_POINT('',(22.,0.75,0.85));
#13952=CARTESIAN_POINT('',(22.,0.75,0.85));
#13953=CARTESIAN_POINT('',(0.,0.75,0.85));
#13954=CARTESIAN_POINT('Origin',(0.,0.75,0.));
#13955=CARTESIAN_POINT('',(0.,0.75,0.));
#13956=CARTESIAN_POINT('',(0.,0.75,0.));
#13957=CARTESIAN_POINT('',(22.,0.75,0.));
#13958=CARTESIAN_POINT('',(22.,0.75,0.));
#13959=CARTESIAN_POINT('',(0.,0.75,0.));
#13960=CARTESIAN_POINT('Origin',(0.,-0.75,0.));
#13961=CARTESIAN_POINT('',(0.,-0.75,0.));
#13962=CARTESIAN_POINT('',(0.,-0.75,0.));
#13963=CARTESIAN_POINT('',(22.,-0.75,0.));
#13964=CARTESIAN_POINT('',(22.,-0.75,0.));
#13965=CARTESIAN_POINT('',(0.,-0.75,0.));
#13966=CARTESIAN_POINT('Origin',(0.,-0.75,0.85));
#13967=CARTESIAN_POINT('',(0.,-0.75,0.85));
#13968=CARTESIAN_POINT('',(22.,-0.75,0.85));
#13969=CARTESIAN_POINT('Origin',(22.,0.,0.75));
#13970=CARTESIAN_POINT('Origin',(0.,0.,0.75));
#13971=CARTESIAN_POINT('',(0.,0.,0.));
#13972=CARTESIAN_POINT('Origin',(0.115470053837925,-0.5,-0.2));
#13973=CARTESIAN_POINT('',(0.23094010767585,-0.5,0.));
#13974=CARTESIAN_POINT('',(0.115470053837925,-0.5,-0.2));
#13975=CARTESIAN_POINT('',(0.23094010767585,-0.5,0.));
#13976=CARTESIAN_POINT('',(0.115470053837925,-0.8,-0.2));
#13977=CARTESIAN_POINT('',(0.115470053837925,-0.5,-0.2));
#13978=CARTESIAN_POINT('',(0.23094010767585,-0.8,0.));
#13979=CARTESIAN_POINT('',(0.23094010767585,-0.8,0.));
#13980=CARTESIAN_POINT('',(0.23094010767585,-0.5,0.));
#13981=CARTESIAN_POINT('Origin',(-0.115470053837925,-0.5,-0.2));
#13982=CARTESIAN_POINT('',(-0.115470053837925,-0.5,-0.2));
#13983=CARTESIAN_POINT('',(0.115470053837925,-0.5,-0.2));
#13984=CARTESIAN_POINT('',(-0.115470053837925,-0.8,-0.2));
#13985=CARTESIAN_POINT('',(-0.115470053837925,-0.5,-0.2));
#13986=CARTESIAN_POINT('',(0.115470053837925,-0.8,-0.2));
#13987=CARTESIAN_POINT('Origin',(-0.23094010767585,-0.5,-2.77555756156289E-17));
#13988=CARTESIAN_POINT('',(-0.23094010767585,-0.5,-2.82820063659975E-17));
#13989=CARTESIAN_POINT('',(-0.115470053837925,-0.5,-0.2));
#13990=CARTESIAN_POINT('',(-0.23094010767585,-0.8,-2.77555756156289E-17));
#13991=CARTESIAN_POINT('',(-0.23094010767585,-0.5,-2.82820063659975E-17));
#13992=CARTESIAN_POINT('',(-0.115470053837925,-0.8,-0.2));
#13993=CARTESIAN_POINT('Origin',(-0.115470053837925,-0.5,0.2));
#13994=CARTESIAN_POINT('',(-0.115470053837925,-0.5,0.2));
#13995=CARTESIAN_POINT('',(-0.23094010767585,-0.5,-2.82820063659975E-17));
#13996=CARTESIAN_POINT('',(-0.115470053837925,-0.8,0.2));
#13997=CARTESIAN_POINT('',(-0.115470053837925,-0.5,0.2));
#13998=CARTESIAN_POINT('',(-0.23094010767585,-0.8,-2.82820063659975E-17));
#13999=CARTESIAN_POINT('Origin',(0.115470053837925,-0.5,0.2));
#14000=CARTESIAN_POINT('',(0.115470053837925,-0.5,0.2));
#14001=CARTESIAN_POINT('',(-0.115470053837925,-0.5,0.2));
#14002=CARTESIAN_POINT('',(0.115470053837925,-0.8,0.2));
#14003=CARTESIAN_POINT('',(0.115470053837925,-0.5,0.2));
#14004=CARTESIAN_POINT('',(-0.115470053837925,-0.8,0.2));
#14005=CARTESIAN_POINT('Origin',(0.23094010767585,-0.5,0.));
#14006=CARTESIAN_POINT('',(0.115470053837925,-0.5,0.2));
#14007=CARTESIAN_POINT('',(0.115470053837925,-0.8,0.2));
#14008=CARTESIAN_POINT('Origin',(0.,-0.5,0.));
#14009=CARTESIAN_POINT('Origin',(0.,-0.8,0.));
#14010=CARTESIAN_POINT('Origin',(0.,-1.9,0.));
#14011=CARTESIAN_POINT('',(-0.25,-1.9,3.06161699786838E-17));
#14012=CARTESIAN_POINT('Origin',(0.,-1.9,0.));
#14013=CARTESIAN_POINT('',(-0.24505,-1.9,3.00099698131059E-17));
#14014=CARTESIAN_POINT('Origin',(0.,-1.9,0.));
#14015=CARTESIAN_POINT('Origin',(0.,-3.,0.));
#14016=CARTESIAN_POINT('',(-0.25,-3.,3.06161699786838E-17));
#14017=CARTESIAN_POINT('',(-0.25,-3.,3.06161699786838E-17));
#14018=CARTESIAN_POINT('Origin',(0.,-3.,0.));
#14019=CARTESIAN_POINT('Origin',(0.,-3.,0.));
#14020=CARTESIAN_POINT('Origin',(0.375,0.5,0.));
#14021=CARTESIAN_POINT('',(-0.375,0.5,-4.59242549680257E-17));
#14022=CARTESIAN_POINT('Origin',(0.,0.5,0.));
#14023=CARTESIAN_POINT('Origin',(0.,0.475,0.));
#14024=CARTESIAN_POINT('',(-0.425,0.45,-5.20474889637625E-17));
#14025=CARTESIAN_POINT('Origin',(0.,0.45,0.));
#14026=CARTESIAN_POINT('',(-0.4,0.475,-4.89858719658941E-17));
#14027=CARTESIAN_POINT('Origin',(0.,0.24,0.));
#14028=CARTESIAN_POINT('',(-0.425,0.0299999999999998,-5.20474889637625E-17));
#14029=CARTESIAN_POINT('Origin',(0.,0.0299999999999998,0.));
#14030=CARTESIAN_POINT('',(-0.425,0.24,-5.20474889637625E-17));
#14031=CARTESIAN_POINT('Origin',(0.,0.0150000000000001,0.));
#14032=CARTESIAN_POINT('',(-0.395,4.85722573273506E-17,-4.83735485663204E-17));
#14033=CARTESIAN_POINT('Origin',(0.,0.,0.));
#14034=CARTESIAN_POINT('',(-0.41,0.0150000000000001,-5.02105187650415E-17));
#14035=CARTESIAN_POINT('Origin',(0.27,0.,0.));
#14036=CARTESIAN_POINT('',(-0.27,0.,-3.30654635769785E-17));
#14037=CARTESIAN_POINT('Origin',(0.,0.,0.));
#14038=CARTESIAN_POINT('Origin',(0.,-0.02,0.));
#14039=CARTESIAN_POINT('',(-0.24505,-0.0498999999999999,3.00099698131059E-17));
#14040=CARTESIAN_POINT('Origin',(0.,-0.0498999999999999,0.));
#14041=CARTESIAN_POINT('',(-0.26,-0.02,-3.18408167778312E-17));
#14042=CARTESIAN_POINT('Origin',(0.,-0.995,0.));
#14043=CARTESIAN_POINT('',(-0.24505,-0.995,-3.00099698131059E-17));
#14044=CARTESIAN_POINT('',(0.,0.,0.));
#14045=CARTESIAN_POINT('Origin',(0.375,0.5,0.));
#14046=CARTESIAN_POINT('',(-0.375,0.5,-4.59242549680257E-17));
#14047=CARTESIAN_POINT('Origin',(0.,0.5,0.));
#14048=CARTESIAN_POINT('Origin',(0.,0.475,0.));
#14049=CARTESIAN_POINT('',(-0.425,0.45,-5.20474889637625E-17));
#14050=CARTESIAN_POINT('Origin',(0.,0.45,0.));
#14051=CARTESIAN_POINT('',(-0.4,0.475,-4.89858719658941E-17));
#14052=CARTESIAN_POINT('Origin',(0.,0.24,0.));
#14053=CARTESIAN_POINT('',(-0.425,0.0299999999999998,-5.20474889637625E-17));
#14054=CARTESIAN_POINT('Origin',(0.,0.0299999999999998,0.));
#14055=CARTESIAN_POINT('',(-0.425,0.24,-5.20474889637625E-17));
#14056=CARTESIAN_POINT('Origin',(0.,0.0150000000000001,0.));
#14057=CARTESIAN_POINT('',(-0.395,4.85722573273506E-17,-4.83735485663204E-17));
#14058=CARTESIAN_POINT('Origin',(0.,0.,0.));
#14059=CARTESIAN_POINT('',(-0.41,0.0150000000000001,-5.02105187650415E-17));
#14060=CARTESIAN_POINT('Origin',(0.27,0.,0.));
#14061=CARTESIAN_POINT('',(-0.27,0.,-3.30654635769785E-17));
#14062=CARTESIAN_POINT('Origin',(0.,0.,0.));
#14063=CARTESIAN_POINT('Origin',(0.,-0.02,0.));
#14064=CARTESIAN_POINT('',(-0.24505,-0.0498999999999999,3.00099698131059E-17));
#14065=CARTESIAN_POINT('Origin',(0.,-0.0498999999999999,0.));
#14066=CARTESIAN_POINT('',(-0.26,-0.02,-3.18408167778312E-17));
#14067=CARTESIAN_POINT('Origin',(0.,-0.995,0.));
#14068=CARTESIAN_POINT('',(-0.24505,-1.95495,3.00099698131059E-17));
#14069=CARTESIAN_POINT('Origin',(0.,-1.95495,0.));
#14070=CARTESIAN_POINT('',(-0.24505,-0.995,-3.00099698131059E-17));
#14071=CARTESIAN_POINT('Origin',(0.,-1.975,0.));
#14072=CARTESIAN_POINT('',(-0.2,-2.,-2.44929359829471E-17));
#14073=CARTESIAN_POINT('Origin',(0.,-2.,0.));
#14074=CARTESIAN_POINT('',(-0.225,-1.975,-2.75545529808154E-17));
#14075=CARTESIAN_POINT('Origin',(0.,-2.,0.));
#14076=CARTESIAN_POINT('Origin',(0.115470053837925,-0.5,-0.2));
#14077=CARTESIAN_POINT('',(0.23094010767585,-0.5,0.));
#14078=CARTESIAN_POINT('',(0.115470053837925,-0.5,-0.2));
#14079=CARTESIAN_POINT('',(0.23094010767585,-0.5,0.));
#14080=CARTESIAN_POINT('',(0.115470053837925,-0.8,-0.2));
#14081=CARTESIAN_POINT('',(0.115470053837925,-0.5,-0.2));
#14082=CARTESIAN_POINT('',(0.23094010767585,-0.8,0.));
#14083=CARTESIAN_POINT('',(0.23094010767585,-0.8,0.));
#14084=CARTESIAN_POINT('',(0.23094010767585,-0.5,0.));
#14085=CARTESIAN_POINT('Origin',(-0.115470053837925,-0.5,-0.2));
#14086=CARTESIAN_POINT('',(-0.115470053837925,-0.5,-0.2));
#14087=CARTESIAN_POINT('',(0.115470053837925,-0.5,-0.2));
#14088=CARTESIAN_POINT('',(-0.115470053837925,-0.8,-0.2));
#14089=CARTESIAN_POINT('',(-0.115470053837925,-0.5,-0.2));
#14090=CARTESIAN_POINT('',(0.115470053837925,-0.8,-0.2));
#14091=CARTESIAN_POINT('Origin',(-0.23094010767585,-0.5,-2.77555756156289E-17));
#14092=CARTESIAN_POINT('',(-0.23094010767585,-0.5,-2.82820063659975E-17));
#14093=CARTESIAN_POINT('',(-0.115470053837925,-0.5,-0.2));
#14094=CARTESIAN_POINT('',(-0.23094010767585,-0.8,-2.77555756156289E-17));
#14095=CARTESIAN_POINT('',(-0.23094010767585,-0.5,-2.82820063659975E-17));
#14096=CARTESIAN_POINT('',(-0.115470053837925,-0.8,-0.2));
#14097=CARTESIAN_POINT('Origin',(-0.115470053837925,-0.5,0.2));
#14098=CARTESIAN_POINT('',(-0.115470053837925,-0.5,0.2));
#14099=CARTESIAN_POINT('',(-0.23094010767585,-0.5,-2.82820063659975E-17));
#14100=CARTESIAN_POINT('',(-0.115470053837925,-0.8,0.2));
#14101=CARTESIAN_POINT('',(-0.115470053837925,-0.5,0.2));
#14102=CARTESIAN_POINT('',(-0.23094010767585,-0.8,-2.82820063659975E-17));
#14103=CARTESIAN_POINT('Origin',(0.115470053837925,-0.5,0.2));
#14104=CARTESIAN_POINT('',(0.115470053837925,-0.5,0.2));
#14105=CARTESIAN_POINT('',(-0.115470053837925,-0.5,0.2));
#14106=CARTESIAN_POINT('',(0.115470053837925,-0.8,0.2));
#14107=CARTESIAN_POINT('',(0.115470053837925,-0.5,0.2));
#14108=CARTESIAN_POINT('',(-0.115470053837925,-0.8,0.2));
#14109=CARTESIAN_POINT('Origin',(0.23094010767585,-0.5,0.));
#14110=CARTESIAN_POINT('',(0.115470053837925,-0.5,0.2));
#14111=CARTESIAN_POINT('',(0.115470053837925,-0.8,0.2));
#14112=CARTESIAN_POINT('Origin',(0.,-0.5,0.));
#14113=CARTESIAN_POINT('Origin',(0.,-0.8,0.));
#14114=CARTESIAN_POINT('',(0.,0.,0.));
#14115=CARTESIAN_POINT('Origin',(0.,0.395,0.25));
#14116=CARTESIAN_POINT('',(-0.5,0.3,0.25));
#14117=CARTESIAN_POINT('',(0.5,0.3,0.25));
#14118=CARTESIAN_POINT('',(0.25,0.3,0.25));
#14119=CARTESIAN_POINT('',(-0.5,0.5,0.25));
#14120=CARTESIAN_POINT('',(-0.5,0.5,0.25));
#14121=CARTESIAN_POINT('',(0.5,0.5,0.25));
#14122=CARTESIAN_POINT('',(0.5,0.5,0.25));
#14123=CARTESIAN_POINT('',(0.5,0.29,0.25));
#14124=CARTESIAN_POINT('Origin',(0.5,0.5,0.25));
#14125=CARTESIAN_POINT('',(-0.5,0.5,0.4));
#14126=CARTESIAN_POINT('',(-0.5,0.5,0.25));
#14127=CARTESIAN_POINT('',(0.5,0.5,0.4));
#14128=CARTESIAN_POINT('',(0.5,0.5,0.4));
#14129=CARTESIAN_POINT('',(0.5,0.5,0.25));
#14130=CARTESIAN_POINT('Origin',(0.,0.,0.4));
#14131=CARTESIAN_POINT('',(-0.5,-0.5,0.4));
#14132=CARTESIAN_POINT('',(-0.5,0.5,0.4));
#14133=CARTESIAN_POINT('',(0.5,-0.5,0.4));
#14134=CARTESIAN_POINT('',(-0.5,-0.5,0.4));
#14135=CARTESIAN_POINT('',(0.5,-0.3,0.4));
#14136=CARTESIAN_POINT('',(-0.2117,2.59257727379495E-17,0.4));
#14137=CARTESIAN_POINT('Origin',(0.,0.,0.4));
#14138=CARTESIAN_POINT('Origin',(-0.5,0.3,0.));
#14139=CARTESIAN_POINT('',(-0.5,0.3,0.15));
#14140=CARTESIAN_POINT('',(-0.5,0.3,0.));
#14141=CARTESIAN_POINT('',(-0.5,0.15,0.));
#14142=CARTESIAN_POINT('',(-0.5,0.225,0.075));
#14143=CARTESIAN_POINT('',(-0.5,-0.15,0.));
#14144=CARTESIAN_POINT('',(-0.5,0.3,0.));
#14145=CARTESIAN_POINT('',(-0.5,-0.3,0.15));
#14146=CARTESIAN_POINT('',(-0.5,-0.075,-0.075));
#14147=CARTESIAN_POINT('',(-0.5,-0.3,0.25));
#14148=CARTESIAN_POINT('',(-0.5,-0.3,0.));
#14149=CARTESIAN_POINT('',(-0.5,-0.5,0.25));
#14150=CARTESIAN_POINT('',(-0.5,-0.29,0.25));
#14151=CARTESIAN_POINT('',(-0.5,-0.5,0.25));
#14152=CARTESIAN_POINT('Origin',(-0.5,-0.5,0.25));
#14153=CARTESIAN_POINT('',(0.5,-0.5,0.25));
#14154=CARTESIAN_POINT('',(-0.5,-0.5,0.25));
#14155=CARTESIAN_POINT('',(0.5,-0.5,0.25));
#14156=CARTESIAN_POINT('Origin',(0.,-0.395,0.25));
#14157=CARTESIAN_POINT('',(0.5,-0.3,0.25));
#14158=CARTESIAN_POINT('',(-0.25,-0.3,0.25));
#14159=CARTESIAN_POINT('',(0.5,-0.5,0.25));
#14160=CARTESIAN_POINT('Origin',(0.5,-0.3,0.));
#14161=CARTESIAN_POINT('',(0.5,-0.3,0.15));
#14162=CARTESIAN_POINT('',(0.5,-0.3,0.));
#14163=CARTESIAN_POINT('',(0.5,-0.15,0.));
#14164=CARTESIAN_POINT('',(0.5,-0.225,0.075));
#14165=CARTESIAN_POINT('',(0.5,0.15,0.));
#14166=CARTESIAN_POINT('',(0.5,-0.3,0.));
#14167=CARTESIAN_POINT('',(0.5,0.3,0.15));
#14168=CARTESIAN_POINT('',(0.5,0.075,-0.075));
#14169=CARTESIAN_POINT('',(0.5,0.3,0.));
#14170=CARTESIAN_POINT('Origin',(-0.5,-0.3,0.));
#14171=CARTESIAN_POINT('',(-0.25,-0.3,0.15));
#14172=CARTESIAN_POINT('Origin',(-0.25,-0.225,0.075));
#14173=CARTESIAN_POINT('',(-0.149388386429468,-0.15,0.));
#14174=CARTESIAN_POINT('',(-0.25,-0.15,0.));
#14175=CARTESIAN_POINT('',(0.149388386429468,-0.15,0.));
#14176=CARTESIAN_POINT('Origin',(0.,0.,-0.15));
#14177=CARTESIAN_POINT('',(-0.25,-0.15,0.));
#14178=CARTESIAN_POINT('Origin',(0.,0.,-0.1));
#14179=CARTESIAN_POINT('',(-0.2117,-2.59257727379495E-17,0.));
#14180=CARTESIAN_POINT('Origin',(0.,0.,0.));
#14181=CARTESIAN_POINT('',(-0.2117,-2.59257727379495E-17,-0.1));
#14182=CARTESIAN_POINT('',(-0.149388386429468,0.15,0.));
#14183=CARTESIAN_POINT('Origin',(0.,0.,0.));
#14184=CARTESIAN_POINT('',(0.149388386429468,0.15,0.));
#14185=CARTESIAN_POINT('Origin',(0.,0.,-0.15));
#14186=CARTESIAN_POINT('Origin',(0.,0.,0.));
#14187=CARTESIAN_POINT('Origin',(0.,0.,0.));
#14188=CARTESIAN_POINT('',(0.25,0.15,0.));
#14189=CARTESIAN_POINT('Origin',(0.,0.,0.));
#14190=CARTESIAN_POINT('',(0.25,0.15,0.));
#14191=CARTESIAN_POINT('Origin',(0.25,0.225,0.075));
#14192=CARTESIAN_POINT('',(0.25,0.3,0.15));
#14193=CARTESIAN_POINT('Origin',(0.5,0.3,0.));
#14194=CARTESIAN_POINT('',(0.,0.,0.));
#14195=CARTESIAN_POINT('Origin',(0.,0.09,0.));
#14196=CARTESIAN_POINT('',(-0.285,0.1,3.49024337756996E-17));
#14197=CARTESIAN_POINT('Origin',(0.,0.1,0.));
#14198=CARTESIAN_POINT('',(-0.265,0.08,-3.24531401774049E-17));
#14199=CARTESIAN_POINT('',(-0.275,0.09,3.36777869765522E-17));
#14200=CARTESIAN_POINT('Origin',(0.,0.08,0.));
#14201=CARTESIAN_POINT('Origin',(0.,0.,0.));
#14202=CARTESIAN_POINT('',(-0.265,0.,3.24531401774049E-17));
#14203=CARTESIAN_POINT('',(-0.265,0.,3.24531401774049E-17));
#14204=CARTESIAN_POINT('Origin',(0.,0.,0.));
#14205=CARTESIAN_POINT('Origin',(0.,0.1,0.));
#14206=CARTESIAN_POINT('',(-0.5,0.1,6.12323399573677E-17));
#14207=CARTESIAN_POINT('Origin',(0.,0.1,0.));
#14208=CARTESIAN_POINT('Origin',(0.,0.,0.));
#14209=CARTESIAN_POINT('',(-0.5,0.,6.12323399573677E-17));
#14210=CARTESIAN_POINT('',(-0.5,0.,6.12323399573677E-17));
#14211=CARTESIAN_POINT('Origin',(0.,0.,0.));
#14212=CARTESIAN_POINT('Origin',(0.,0.,0.));
#14213=CARTESIAN_POINT('',(0.,0.,0.));
#14214=CARTESIAN_POINT('',(0.,0.,0.));
#14215=CARTESIAN_POINT('Origin',(-2.1,3.,17.6));
#14216=CARTESIAN_POINT('',(-2.,3.,17.825));
#14217=CARTESIAN_POINT('Origin',(-2.,3.,17.6));
#14218=CARTESIAN_POINT('',(-1.2,3.,17.825));
#14219=CARTESIAN_POINT('',(-2.1,3.,17.825));
#14220=CARTESIAN_POINT('Origin',(-1.2,3.,17.6));
#14221=CARTESIAN_POINT('Origin',(-1.6,3.,17.));
#14222=CARTESIAN_POINT('',(-2.,3.,17.));
#14223=CARTESIAN_POINT('',(-1.2,3.,17.));
#14224=CARTESIAN_POINT('',(-1.4,3.,17.));
#14225=CARTESIAN_POINT('',(-2.,3.6,17.));
#14226=CARTESIAN_POINT('',(-2.,3.6,17.));
#14227=CARTESIAN_POINT('',(-1.2,3.6,17.));
#14228=CARTESIAN_POINT('',(-1.2,3.6,17.));
#14229=CARTESIAN_POINT('',(-1.2,2.4,17.));
#14230=CARTESIAN_POINT('Origin',(-1.2,3.6,17.));
#14231=CARTESIAN_POINT('',(-2.,3.6,18.2));
#14232=CARTESIAN_POINT('',(-2.,3.6,17.));
#14233=CARTESIAN_POINT('',(-1.2,3.6,18.2));
#14234=CARTESIAN_POINT('',(-1.2,3.6,18.2));
#14235=CARTESIAN_POINT('',(-1.2,3.6,17.));
#14236=CARTESIAN_POINT('Origin',(-1.6,3.,18.2));
#14237=CARTESIAN_POINT('',(-1.2,3.,18.2));
#14238=CARTESIAN_POINT('',(-2.,3.,18.2));
#14239=CARTESIAN_POINT('',(-1.4,3.,18.2));
#14240=CARTESIAN_POINT('',(-1.2,2.4,18.2));
#14241=CARTESIAN_POINT('',(-2.,3.6,18.2));
#14242=CARTESIAN_POINT('Origin',(-1.2,3.,16.));
#14243=CARTESIAN_POINT('',(-1.2,3.,16.));
#14244=CARTESIAN_POINT('',(-1.2,3.,16.));
#14245=CARTESIAN_POINT('',(-2.,3.,16.));
#14246=CARTESIAN_POINT('',(-1.2,3.,16.));
#14247=CARTESIAN_POINT('',(-2.,3.,16.));
#14248=CARTESIAN_POINT('Origin',(-1.2,3.,16.));
#14249=CARTESIAN_POINT('',(-2.,3.,21.));
#14250=CARTESIAN_POINT('',(-2.,3.,16.));
#14251=CARTESIAN_POINT('',(-2.,3.,22.));
#14252=CARTESIAN_POINT('',(-2.,3.,16.));
#14253=CARTESIAN_POINT('',(-2.,3.,23.));
#14254=CARTESIAN_POINT('',(-2.,3.,16.));
#14255=CARTESIAN_POINT('',(-1.2,3.,23.));
#14256=CARTESIAN_POINT('',(-1.2,3.,23.));
#14257=CARTESIAN_POINT('',(-1.2,3.,16.));
#14258=CARTESIAN_POINT('Origin',(-7.,0.,20.9));
#14259=CARTESIAN_POINT('',(-7.525,-6.42939569552361E-17,21.));
#14260=CARTESIAN_POINT('Origin',(-7.,0.,21.));
#14261=CARTESIAN_POINT('',(-7.525,6.42939569552361E-17,22.));
#14262=CARTESIAN_POINT('',(-7.525,-6.42939569552361E-17,20.9));
#14263=CARTESIAN_POINT('Origin',(-7.,0.,22.));
#14264=CARTESIAN_POINT('Origin',(-5.2,0.,20.9));
#14265=CARTESIAN_POINT('',(-5.65,-5.51091059616309E-17,21.));
#14266=CARTESIAN_POINT('Origin',(-5.2,0.,21.));
#14267=CARTESIAN_POINT('',(-5.65,5.51091059616309E-17,22.));
#14268=CARTESIAN_POINT('',(-5.65,-5.51091059616309E-17,20.9));
#14269=CARTESIAN_POINT('Origin',(-5.2,0.,22.));
#14270=CARTESIAN_POINT('Origin',(-8.8,0.,20.9));
#14271=CARTESIAN_POINT('',(-9.25,-5.51091059616308E-17,21.));
#14272=CARTESIAN_POINT('Origin',(-8.8,0.,21.));
#14273=CARTESIAN_POINT('',(-9.25,5.51091059616308E-17,22.));
#14274=CARTESIAN_POINT('',(-9.25,-5.51091059616308E-17,20.9));
#14275=CARTESIAN_POINT('Origin',(-8.8,0.,22.));
#14276=CARTESIAN_POINT('Origin',(-2.7,1.9,21.));
#14277=CARTESIAN_POINT('',(-2.7,1.4,21.));
#14278=CARTESIAN_POINT('',(-2.,1.4,21.));
#14279=CARTESIAN_POINT('',(-2.7,1.4,21.));
#14280=CARTESIAN_POINT('',(-2.7,2.4,21.));
#14281=CARTESIAN_POINT('Origin',(-2.7,1.9,21.));
#14282=CARTESIAN_POINT('',(-2.,2.4,21.));
#14283=CARTESIAN_POINT('',(-2.7,2.4,21.));
#14284=CARTESIAN_POINT('Origin',(-2.,1.9,21.));
#14285=CARTESIAN_POINT('Origin',(-2.7,1.9,21.));
#14286=CARTESIAN_POINT('',(-2.7,0.95,21.));
#14287=CARTESIAN_POINT('Origin',(-2.,3.,16.));
#14288=CARTESIAN_POINT('',(-2.,-3.,16.));
#14289=CARTESIAN_POINT('',(-2.,3.,16.));
#14290=CARTESIAN_POINT('',(-2.,-3.,21.));
#14291=CARTESIAN_POINT('',(-2.,-3.,16.));
#14292=CARTESIAN_POINT('',(-2.,-2.4,21.));
#14293=CARTESIAN_POINT('',(-2.,1.5,21.));
#14294=CARTESIAN_POINT('',(-2.,-1.4,21.));
#14295=CARTESIAN_POINT('Origin',(-2.,-1.9,21.));
#14296=CARTESIAN_POINT('',(-2.,1.5,21.));
#14297=CARTESIAN_POINT('',(-2.,1.5,21.));
#14298=CARTESIAN_POINT('',(-2.,1.9,21.275));
#14299=CARTESIAN_POINT('Origin',(-2.,1.9,21.));
#14300=CARTESIAN_POINT('',(-2.,-1.9,18.275));
#14301=CARTESIAN_POINT('Origin',(-2.,-1.9,18.));
#14302=CARTESIAN_POINT('',(-2.,-1.9,21.275));
#14303=CARTESIAN_POINT('Origin',(-2.,-1.9,21.));
#14304=CARTESIAN_POINT('',(-2.,1.9,18.275));
#14305=CARTESIAN_POINT('Origin',(-2.,1.9,18.));
#14306=CARTESIAN_POINT('Origin',(-2.1,1.9,21.));
#14307=CARTESIAN_POINT('',(-1.2,1.9,21.275));
#14308=CARTESIAN_POINT('',(-2.1,1.9,21.275));
#14309=CARTESIAN_POINT('Origin',(-1.2,1.9,21.));
#14310=CARTESIAN_POINT('Origin',(-7.,0.,21.));
#14311=CARTESIAN_POINT('',(-2.7,-1.4,21.));
#14312=CARTESIAN_POINT('',(-2.7,-1.4,21.));
#14313=CARTESIAN_POINT('',(-2.7,-2.4,21.));
#14314=CARTESIAN_POINT('',(-2.7,-0.95,21.));
#14315=CARTESIAN_POINT('',(-2.7,-2.4,21.));
#14316=CARTESIAN_POINT('',(-2.,-6.,21.));
#14317=CARTESIAN_POINT('',(-2.,-6.,21.));
#14318=CARTESIAN_POINT('',(-12.,-6.,21.));
#14319=CARTESIAN_POINT('',(-12.,-6.,21.));
#14320=CARTESIAN_POINT('',(-12.,6.,21.));
#14321=CARTESIAN_POINT('',(-12.,6.,21.));
#14322=CARTESIAN_POINT('',(-2.,6.,21.));
#14323=CARTESIAN_POINT('',(-2.,6.,21.));
#14324=CARTESIAN_POINT('',(-2.,-6.,21.));
#14325=CARTESIAN_POINT('Origin',(-2.1,1.9,18.));
#14326=CARTESIAN_POINT('',(-1.2,1.9,18.275));
#14327=CARTESIAN_POINT('',(-2.1,1.9,18.275));
#14328=CARTESIAN_POINT('Origin',(-1.2,1.9,18.));
#14329=CARTESIAN_POINT('Origin',(-2.7,-1.9,21.));
#14330=CARTESIAN_POINT('Origin',(-2.7,-1.9,21.));
#14331=CARTESIAN_POINT('Origin',(-2.7,-1.9,21.));
#14332=CARTESIAN_POINT('Origin',(-2.1,-1.9,21.));
#14333=CARTESIAN_POINT('',(-1.2,-1.9,21.275));
#14334=CARTESIAN_POINT('',(-2.1,-1.9,21.275));
#14335=CARTESIAN_POINT('Origin',(-1.2,-1.9,21.));
#14336=CARTESIAN_POINT('Origin',(-2.1,-1.9,18.));
#14337=CARTESIAN_POINT('',(-1.2,-1.9,18.275));
#14338=CARTESIAN_POINT('',(-2.1,-1.9,18.275));
#14339=CARTESIAN_POINT('Origin',(-1.2,-1.9,18.));
#14340=CARTESIAN_POINT('Origin',(-2.,-6.,21.));
#14341=CARTESIAN_POINT('',(-2.,-3.,22.));
#14342=CARTESIAN_POINT('',(-2.,-3.,16.));
#14343=CARTESIAN_POINT('',(-2.,-6.,22.));
#14344=CARTESIAN_POINT('',(-2.,-6.,22.));
#14345=CARTESIAN_POINT('',(-2.,-6.,21.));
#14346=CARTESIAN_POINT('Origin',(-2.,-6.,21.));
#14347=CARTESIAN_POINT('',(-2.,6.,22.));
#14348=CARTESIAN_POINT('',(-2.,6.,21.));
#14349=CARTESIAN_POINT('',(-2.,-6.,22.));
#14350=CARTESIAN_POINT('Origin',(-2.,6.,21.));
#14351=CARTESIAN_POINT('',(-12.,6.,22.));
#14352=CARTESIAN_POINT('',(-12.,6.,21.));
#14353=CARTESIAN_POINT('',(-2.,6.,22.));
#14354=CARTESIAN_POINT('Origin',(-12.,-6.,21.));
#14355=CARTESIAN_POINT('',(-12.,-6.,22.));
#14356=CARTESIAN_POINT('',(-12.,-6.,22.));
#14357=CARTESIAN_POINT('',(-12.,-6.,21.));
#14358=CARTESIAN_POINT('Origin',(-12.,6.,21.));
#14359=CARTESIAN_POINT('',(-12.,6.,22.));
#14360=CARTESIAN_POINT('Origin',(-7.,0.,22.));
#14361=CARTESIAN_POINT('',(-2.,1.5,22.));
#14362=CARTESIAN_POINT('Origin',(-2.,3.,16.));
#14363=CARTESIAN_POINT('',(-2.,-3.,23.));
#14364=CARTESIAN_POINT('',(-2.,-3.,16.));
#14365=CARTESIAN_POINT('',(-2.,3.,23.));
#14366=CARTESIAN_POINT('Origin',(-1.2,-3.,16.));
#14367=CARTESIAN_POINT('',(-1.2,-3.,23.));
#14368=CARTESIAN_POINT('',(-1.2,-3.,23.));
#14369=CARTESIAN_POINT('',(-1.2,-3.,16.));
#14370=CARTESIAN_POINT('',(-1.2,-3.,16.));
#14371=CARTESIAN_POINT('',(-1.2,-3.,16.));
#14372=CARTESIAN_POINT('Origin',(-2.,-3.,16.));
#14373=CARTESIAN_POINT('',(-2.,-3.,16.));
#14374=CARTESIAN_POINT('',(-2.,-3.,23.));
#14375=CARTESIAN_POINT('Origin',(-1.6,0.,23.));
#14376=CARTESIAN_POINT('Origin',(-1.6,0.,16.));
#14377=CARTESIAN_POINT('',(0.,0.,0.));
#14378=CARTESIAN_POINT('Origin',(-7.,0.,4.9));
#14379=CARTESIAN_POINT('',(-7.425,-5.20474889637625E-17,5.));
#14380=CARTESIAN_POINT('Origin',(-7.,0.,5.));
#14381=CARTESIAN_POINT('',(-7.425,5.20474889637625E-17,5.5));
#14382=CARTESIAN_POINT('',(-7.425,-5.20474889637625E-17,4.9));
#14383=CARTESIAN_POINT('Origin',(-7.,0.,5.5));
#14384=CARTESIAN_POINT('Origin',(-7.,0.,5.));
#14385=CARTESIAN_POINT('',(-8.09,-1.33486501107061E-16,5.5));
#14386=CARTESIAN_POINT('Origin',(-7.,0.,5.5));
#14387=CARTESIAN_POINT('',(-8.09,-1.33486501107061E-16,5.));
#14388=CARTESIAN_POINT('',(-8.09,-1.33486501107061E-16,5.));
#14389=CARTESIAN_POINT('Origin',(-7.,0.,5.));
#14390=CARTESIAN_POINT('Origin',(-7.,0.,5.5));
#14391=CARTESIAN_POINT('Origin',(-7.,0.,5.));
#14392=CARTESIAN_POINT('',(0.,0.,0.));
#14393=CARTESIAN_POINT('Origin',(-7.,0.,21.));
#14394=CARTESIAN_POINT('',(-7.5,-6.12323399573677E-17,23.));
#14395=CARTESIAN_POINT('Origin',(-7.,0.,23.));
#14396=CARTESIAN_POINT('',(-7.5,-6.12323399573677E-17,21.));
#14397=CARTESIAN_POINT('',(-7.5,-6.12323399573677E-17,21.));
#14398=CARTESIAN_POINT('Origin',(-7.,0.,21.));
#14399=CARTESIAN_POINT('Origin',(-7.,0.,23.));
#14400=CARTESIAN_POINT('Origin',(-7.,0.,4.5));
#14401=CARTESIAN_POINT('',(-7.5,-6.12323399573677E-17,5.5));
#14402=CARTESIAN_POINT('Origin',(-7.,0.,5.5));
#14403=CARTESIAN_POINT('',(-7.5,-6.12323399573677E-17,4.5));
#14404=CARTESIAN_POINT('',(-7.5,-6.12323399573677E-17,4.5));
#14405=CARTESIAN_POINT('Origin',(-7.,0.,4.5));
#14406=CARTESIAN_POINT('Origin',(-7.,0.,4.5));
#14407=CARTESIAN_POINT('Origin',(-7.,0.,20.5));
#14408=CARTESIAN_POINT('',(-8.,-1.22464679914735E-16,20.5));
#14409=CARTESIAN_POINT('Origin',(-7.,0.,20.5));
#14410=CARTESIAN_POINT('',(-7.6,-7.34788079488412E-17,20.5));
#14411=CARTESIAN_POINT('Origin',(-7.,0.,20.5));
#14412=CARTESIAN_POINT('Origin',(-7.,0.,20.5));
#14413=CARTESIAN_POINT('',(-8.,-1.22464679914735E-16,21.));
#14414=CARTESIAN_POINT('Origin',(-7.,0.,21.));
#14415=CARTESIAN_POINT('',(-8.,-1.22464679914735E-16,20.5));
#14416=CARTESIAN_POINT('Origin',(-7.,0.,21.));
#14417=CARTESIAN_POINT('Origin',(-7.,0.,5.5));
#14418=CARTESIAN_POINT('',(-7.6,-7.34788079488412E-17,5.5));
#14419=CARTESIAN_POINT('',(-7.6,-7.34788079488412E-17,5.5));
#14420=CARTESIAN_POINT('Origin',(-7.,0.,5.5));
#14421=CARTESIAN_POINT('Origin',(-7.,0.,5.5));
#14422=CARTESIAN_POINT('',(0.,0.,0.));
#14423=CARTESIAN_POINT('Origin',(-7.,0.,22.));
#14424=CARTESIAN_POINT('',(-7.425,-5.20474889637625E-17,22.8));
#14425=CARTESIAN_POINT('Origin',(-7.,0.,22.8));
#14426=CARTESIAN_POINT('',(-7.425,-5.20474889637625E-17,22.));
#14427=CARTESIAN_POINT('',(-7.425,-5.20474889637625E-17,22.));
#14428=CARTESIAN_POINT('Origin',(-7.,0.,22.));
#14429=CARTESIAN_POINT('Origin',(-7.,0.,22.));
#14430=CARTESIAN_POINT('',(-7.9,-1.10218211923262E-16,22.8));
#14431=CARTESIAN_POINT('Origin',(-7.,0.,22.8));
#14432=CARTESIAN_POINT('',(-7.9,-1.10218211923262E-16,22.));
#14433=CARTESIAN_POINT('',(-7.9,-1.10218211923262E-16,22.));
#14434=CARTESIAN_POINT('Origin',(-7.,0.,22.));
#14435=CARTESIAN_POINT('Origin',(-7.,0.,22.8));
#14436=CARTESIAN_POINT('Origin',(-7.,0.,22.));
#14437=CARTESIAN_POINT('',(0.,0.,0.));
#14438=CARTESIAN_POINT('Origin',(1.8,-0.1,17.6));
#14439=CARTESIAN_POINT('',(1.55,2.4,17.6));
#14440=CARTESIAN_POINT('Origin',(1.8,2.4,17.6));
#14441=CARTESIAN_POINT('',(1.55,3.6,17.6));
#14442=CARTESIAN_POINT('',(1.55,-0.1,17.6));
#14443=CARTESIAN_POINT('Origin',(1.8,3.6,17.6));
#14444=CARTESIAN_POINT('Origin',(-1.3,3.,17.6));
#14445=CARTESIAN_POINT('',(-1.2,3.,17.765));
#14446=CARTESIAN_POINT('Origin',(-1.2,3.,17.6));
#14447=CARTESIAN_POINT('',(-0.0999999999999999,3.,17.765));
#14448=CARTESIAN_POINT('',(-1.3,3.,17.765));
#14449=CARTESIAN_POINT('Origin',(-0.0999999999999999,3.,17.6));
#14450=CARTESIAN_POINT('Origin',(-0.0999999999999999,3.,17.6));
#14451=CARTESIAN_POINT('Origin',(2.4,3.6,17.));
#14452=CARTESIAN_POINT('',(2.4,3.6,17.));
#14453=CARTESIAN_POINT('',(-1.2,3.6,17.));
#14454=CARTESIAN_POINT('',(2.4,3.6,17.));
#14455=CARTESIAN_POINT('',(-1.2,3.6,18.2));
#14456=CARTESIAN_POINT('',(-1.2,3.6,17.));
#14457=CARTESIAN_POINT('',(2.4,3.6,18.2));
#14458=CARTESIAN_POINT('',(2.4,3.6,18.2));
#14459=CARTESIAN_POINT('',(2.4,3.6,17.));
#14460=CARTESIAN_POINT('Origin',(2.4,2.4,17.));
#14461=CARTESIAN_POINT('',(2.4,2.4,17.));
#14462=CARTESIAN_POINT('',(2.4,2.4,17.));
#14463=CARTESIAN_POINT('',(2.4,2.4,18.2));
#14464=CARTESIAN_POINT('',(2.4,2.4,18.2));
#14465=CARTESIAN_POINT('',(2.4,2.4,17.));
#14466=CARTESIAN_POINT('Origin',(-1.2,2.4,17.));
#14467=CARTESIAN_POINT('',(-1.2,2.4,17.));
#14468=CARTESIAN_POINT('',(-1.2,2.4,17.));
#14469=CARTESIAN_POINT('',(-1.2,2.4,18.2));
#14470=CARTESIAN_POINT('',(-1.2,2.4,18.2));
#14471=CARTESIAN_POINT('',(-1.2,2.4,17.));
#14472=CARTESIAN_POINT('Origin',(-1.2,3.6,17.));
#14473=CARTESIAN_POINT('',(-1.2,3.6,17.));
#14474=CARTESIAN_POINT('',(-1.2,3.6,18.2));
#14475=CARTESIAN_POINT('Origin',(0.6,3.,18.2));
#14476=CARTESIAN_POINT('Origin',(0.6,3.,17.));
#14477=CARTESIAN_POINT('',(0.,0.,0.));
#14478=CARTESIAN_POINT('Origin',(2.2,1.8,17.2));
#14479=CARTESIAN_POINT('',(2.2,1.8,17.2));
#14480=CARTESIAN_POINT('',(1.4,1.8,17.2));
#14481=CARTESIAN_POINT('',(2.2,1.8,17.2));
#14482=CARTESIAN_POINT('',(1.4,1.8,18.));
#14483=CARTESIAN_POINT('',(1.4,1.8,17.2));
#14484=CARTESIAN_POINT('',(2.2,1.8,18.));
#14485=CARTESIAN_POINT('',(2.2,1.8,18.));
#14486=CARTESIAN_POINT('',(2.2,1.8,17.2));
#14487=CARTESIAN_POINT('Origin',(2.2,1.2,17.2));
#14488=CARTESIAN_POINT('',(2.2,1.2,17.2));
#14489=CARTESIAN_POINT('',(2.2,1.2,17.2));
#14490=CARTESIAN_POINT('',(2.2,1.2,18.));
#14491=CARTESIAN_POINT('',(2.2,1.2,18.));
#14492=CARTESIAN_POINT('',(2.2,1.2,17.2));
#14493=CARTESIAN_POINT('Origin',(1.4,1.2,17.2));
#14494=CARTESIAN_POINT('',(1.4,1.2,17.2));
#14495=CARTESIAN_POINT('',(1.4,1.2,17.2));
#14496=CARTESIAN_POINT('',(1.4,1.2,18.));
#14497=CARTESIAN_POINT('',(1.4,1.2,18.));
#14498=CARTESIAN_POINT('',(1.4,1.2,17.2));
#14499=CARTESIAN_POINT('Origin',(1.4,1.8,17.2));
#14500=CARTESIAN_POINT('',(1.4,1.8,17.2));
#14501=CARTESIAN_POINT('',(1.4,1.8,18.));
#14502=CARTESIAN_POINT('Origin',(1.8,1.5,18.));
#14503=CARTESIAN_POINT('Origin',(1.8,1.5,17.2));
#14504=CARTESIAN_POINT('',(0.,0.,0.));
#14505=CARTESIAN_POINT('Origin',(1.8,3.6,17.6));
#14506=CARTESIAN_POINT('',(0.6,4.4,17.6));
#14507=CARTESIAN_POINT('Origin',(1.8,4.4,17.6));
#14508=CARTESIAN_POINT('',(0.6,3.6,17.6));
#14509=CARTESIAN_POINT('',(0.6,3.6,17.6));
#14510=CARTESIAN_POINT('Origin',(1.8,3.6,17.6));
#14511=CARTESIAN_POINT('Origin',(1.8,4.4,17.6));
#14512=CARTESIAN_POINT('Origin',(1.8,3.6,17.6));
#14513=CARTESIAN_POINT('',(1.5,3.6,17.6));
#14514=CARTESIAN_POINT('Origin',(1.8,3.6,17.6));
#14515=CARTESIAN_POINT('Origin',(1.8,1.8,17.6));
#14516=CARTESIAN_POINT('',(1.5,1.8,17.6));
#14517=CARTESIAN_POINT('',(1.5,1.8,17.6));
#14518=CARTESIAN_POINT('Origin',(1.8,1.8,17.6));
#14519=CARTESIAN_POINT('Origin',(1.8,1.8,17.6));
#14520=CARTESIAN_POINT('',(0.,0.,0.));
#14521=CARTESIAN_POINT('',(0.,0.,0.));
#14522=CARTESIAN_POINT('Origin',(1.5,-1.9,1.7));
#14523=CARTESIAN_POINT('',(1.56403124237433,-1.7,1.7));
#14524=CARTESIAN_POINT('',(1.43596875762567,-1.7,1.7));
#14525=CARTESIAN_POINT('',(0.75,-1.7,1.7));
#14526=CARTESIAN_POINT('Origin',(1.5,-1.9,1.7));
#14527=CARTESIAN_POINT('Origin',(1.5,-1.9,1.7));
#14528=CARTESIAN_POINT('',(1.56403124237433,-1.7,1.75));
#14529=CARTESIAN_POINT('',(1.56403124237433,-1.7,1.7));
#14530=CARTESIAN_POINT('',(1.29,-1.9,1.75));
#14531=CARTESIAN_POINT('Origin',(1.5,-1.9,1.75));
#14532=CARTESIAN_POINT('',(1.29,-1.9,2.4));
#14533=CARTESIAN_POINT('',(1.29,-1.9,1.7));
#14534=CARTESIAN_POINT('Origin',(1.5,-1.9,2.4));
#14535=CARTESIAN_POINT('',(1.43596875762567,-1.7,1.75));
#14536=CARTESIAN_POINT('Origin',(1.5,-1.9,1.75));
#14537=CARTESIAN_POINT('',(1.43596875762567,-1.7,1.7));
#14538=CARTESIAN_POINT('Origin',(-1.5,1.9,1.7));
#14539=CARTESIAN_POINT('',(-1.56403124237433,1.7,1.7));
#14540=CARTESIAN_POINT('',(-1.43596875762567,1.7,1.7));
#14541=CARTESIAN_POINT('',(-0.75,1.7,1.7));
#14542=CARTESIAN_POINT('Origin',(-1.5,1.9,1.7));
#14543=CARTESIAN_POINT('Origin',(-1.5,1.9,1.7));
#14544=CARTESIAN_POINT('',(-1.56403124237433,1.7,1.75));
#14545=CARTESIAN_POINT('',(-1.56403124237433,1.7,1.7));
#14546=CARTESIAN_POINT('',(-1.71,1.9,1.75));
#14547=CARTESIAN_POINT('Origin',(-1.5,1.9,1.75));
#14548=CARTESIAN_POINT('',(-1.71,1.9,2.4));
#14549=CARTESIAN_POINT('',(-1.71,1.9,1.7));
#14550=CARTESIAN_POINT('Origin',(-1.5,1.9,2.4));
#14551=CARTESIAN_POINT('',(-1.43596875762567,1.7,1.75));
#14552=CARTESIAN_POINT('Origin',(-1.5,1.9,1.75));
#14553=CARTESIAN_POINT('',(-1.43596875762567,1.7,1.7));
#14554=CARTESIAN_POINT('Origin',(-1.5,-1.9,1.7));
#14555=CARTESIAN_POINT('',(-1.43596875762567,-1.7,1.7));
#14556=CARTESIAN_POINT('',(-1.56403124237433,-1.7,1.7));
#14557=CARTESIAN_POINT('',(-0.75,-1.7,1.7));
#14558=CARTESIAN_POINT('Origin',(-1.5,-1.9,1.7));
#14559=CARTESIAN_POINT('Origin',(-1.5,-1.9,1.7));
#14560=CARTESIAN_POINT('',(-1.43596875762567,-1.7,1.75));
#14561=CARTESIAN_POINT('',(-1.43596875762567,-1.7,1.7));
#14562=CARTESIAN_POINT('',(-1.71,-1.9,1.75));
#14563=CARTESIAN_POINT('Origin',(-1.5,-1.9,1.75));
#14564=CARTESIAN_POINT('',(-1.71,-1.9,2.4));
#14565=CARTESIAN_POINT('',(-1.71,-1.9,1.7));
#14566=CARTESIAN_POINT('Origin',(-1.5,-1.9,2.4));
#14567=CARTESIAN_POINT('',(-1.56403124237433,-1.7,1.75));
#14568=CARTESIAN_POINT('Origin',(-1.5,-1.9,1.75));
#14569=CARTESIAN_POINT('',(-1.56403124237433,-1.7,1.7));
#14570=CARTESIAN_POINT('Origin',(1.5,1.9,1.7));
#14571=CARTESIAN_POINT('',(1.43596875762567,1.7,1.7));
#14572=CARTESIAN_POINT('',(1.56403124237433,1.7,1.7));
#14573=CARTESIAN_POINT('',(0.75,1.7,1.7));
#14574=CARTESIAN_POINT('Origin',(1.5,1.9,1.7));
#14575=CARTESIAN_POINT('Origin',(1.5,1.9,1.7));
#14576=CARTESIAN_POINT('',(1.43596875762567,1.7,1.75));
#14577=CARTESIAN_POINT('',(1.43596875762567,1.7,1.7));
#14578=CARTESIAN_POINT('',(1.29,1.9,1.75));
#14579=CARTESIAN_POINT('Origin',(1.5,1.9,1.75));
#14580=CARTESIAN_POINT('',(1.29,1.9,2.4));
#14581=CARTESIAN_POINT('',(1.29,1.9,1.7));
#14582=CARTESIAN_POINT('Origin',(1.5,1.9,2.4));
#14583=CARTESIAN_POINT('',(1.56403124237433,1.7,1.75));
#14584=CARTESIAN_POINT('Origin',(1.5,1.9,1.75));
#14585=CARTESIAN_POINT('',(1.56403124237433,1.7,1.7));
#14586=CARTESIAN_POINT('Origin',(0.,-1.7,1.75));
#14587=CARTESIAN_POINT('',(0.,-1.7,1.75));
#14588=CARTESIAN_POINT('',(-1.97,-1.7,1.75));
#14589=CARTESIAN_POINT('',(0.,-1.7,1.75));
#14590=CARTESIAN_POINT('',(-1.97,-1.7,0.43));
#14591=CARTESIAN_POINT('',(-1.97,-1.7,1.75));
#14592=CARTESIAN_POINT('',(1.97,-1.7,0.43));
#14593=CARTESIAN_POINT('',(0.,-1.7,0.43));
#14594=CARTESIAN_POINT('',(1.97,-1.7,1.75));
#14595=CARTESIAN_POINT('',(1.97,-1.7,1.75));
#14596=CARTESIAN_POINT('',(0.,-1.7,1.75));
#14597=CARTESIAN_POINT('Origin',(0.,1.7,0.43));
#14598=CARTESIAN_POINT('',(0.,1.7,1.75));
#14599=CARTESIAN_POINT('',(1.97,1.7,1.75));
#14600=CARTESIAN_POINT('',(0.,1.7,1.75));
#14601=CARTESIAN_POINT('',(1.97,1.7,0.43));
#14602=CARTESIAN_POINT('',(1.97,1.7,0.43));
#14603=CARTESIAN_POINT('',(-1.97,1.7,0.43));
#14604=CARTESIAN_POINT('',(0.,1.7,0.43));
#14605=CARTESIAN_POINT('',(-1.97,1.7,1.75));
#14606=CARTESIAN_POINT('',(-1.97,1.7,0.43));
#14607=CARTESIAN_POINT('',(0.,1.7,1.75));
#14608=CARTESIAN_POINT('Origin',(-1.97,0.,1.415));
#14609=CARTESIAN_POINT('',(-1.97,-2.35,1.75));
#14610=CARTESIAN_POINT('',(-1.97,-2.35,1.75));
#14611=CARTESIAN_POINT('',(-1.97,-2.35,2.4));
#14612=CARTESIAN_POINT('',(-1.97,-2.35,2.4));
#14613=CARTESIAN_POINT('',(-1.97,2.35,2.4));
#14614=CARTESIAN_POINT('',(-1.97,2.35,2.4));
#14615=CARTESIAN_POINT('',(-1.97,2.35,1.75));
#14616=CARTESIAN_POINT('',(-1.97,2.35,1.75));
#14617=CARTESIAN_POINT('',(-1.97,1.7,1.75));
#14618=CARTESIAN_POINT('',(-1.97,0.78,0.43));
#14619=CARTESIAN_POINT('',(-1.97,0.78,0.43));
#14620=CARTESIAN_POINT('',(-1.97,0.78,1.55));
#14621=CARTESIAN_POINT('',(-1.97,0.78,1.55));
#14622=CARTESIAN_POINT('',(-1.97,-0.78,1.55));
#14623=CARTESIAN_POINT('',(-1.97,-0.78,1.55));
#14624=CARTESIAN_POINT('',(-1.97,-0.78,0.43));
#14625=CARTESIAN_POINT('',(-1.97,-0.78,0.43));
#14626=CARTESIAN_POINT('',(-1.97,-1.7,0.43));
#14627=CARTESIAN_POINT('Origin',(0.,-2.35,1.75));
#14628=CARTESIAN_POINT('',(1.97,-2.35,1.75));
#14629=CARTESIAN_POINT('',(1.97,-2.35,1.75));
#14630=CARTESIAN_POINT('',(0.,-2.35,1.75));
#14631=CARTESIAN_POINT('Origin',(0.,-2.35,2.4));
#14632=CARTESIAN_POINT('',(1.97,-2.35,2.4));
#14633=CARTESIAN_POINT('',(1.97,-2.35,2.4));
#14634=CARTESIAN_POINT('',(0.,-2.35,2.4));
#14635=CARTESIAN_POINT('Origin',(0.,2.35,2.4));
#14636=CARTESIAN_POINT('',(1.97,2.35,2.4));
#14637=CARTESIAN_POINT('',(1.97,2.35,2.4));
#14638=CARTESIAN_POINT('',(0.,2.35,2.4));
#14639=CARTESIAN_POINT('Origin',(0.,2.35,1.75));
#14640=CARTESIAN_POINT('',(1.97,2.35,1.75));
#14641=CARTESIAN_POINT('',(1.97,2.35,1.75));
#14642=CARTESIAN_POINT('',(0.,2.35,1.75));
#14643=CARTESIAN_POINT('Origin',(0.,1.7,1.75));
#14644=CARTESIAN_POINT('',(1.97,1.7,1.75));
#14645=CARTESIAN_POINT('Origin',(0.,0.78,0.43));
#14646=CARTESIAN_POINT('',(1.97,0.78,0.43));
#14647=CARTESIAN_POINT('',(1.97,0.78,0.43));
#14648=CARTESIAN_POINT('',(0.,0.78,0.43));
#14649=CARTESIAN_POINT('Origin',(0.,0.78,1.55));
#14650=CARTESIAN_POINT('',(1.97,0.78,1.55));
#14651=CARTESIAN_POINT('',(1.97,0.78,1.55));
#14652=CARTESIAN_POINT('',(0.,0.78,1.55));
#14653=CARTESIAN_POINT('Origin',(0.,-0.78,1.55));
#14654=CARTESIAN_POINT('',(1.97,-0.78,1.55));
#14655=CARTESIAN_POINT('',(1.97,-0.78,1.55));
#14656=CARTESIAN_POINT('',(0.,-0.78,1.55));
#14657=CARTESIAN_POINT('Origin',(0.,-0.78,0.43));
#14658=CARTESIAN_POINT('',(1.97,-0.78,0.43));
#14659=CARTESIAN_POINT('',(1.97,-0.78,0.43));
#14660=CARTESIAN_POINT('',(0.,-0.78,0.43));
#14661=CARTESIAN_POINT('Origin',(0.,-1.7,0.43));
#14662=CARTESIAN_POINT('',(1.97,-1.7,0.43));
#14663=CARTESIAN_POINT('Origin',(1.97,0.,1.415));
#14664=CARTESIAN_POINT('',(0.,0.,0.));
#14665=CARTESIAN_POINT('Origin',(1.97,1.7,2.3));
#14666=CARTESIAN_POINT('',(1.97,1.7,2.3));
#14667=CARTESIAN_POINT('',(1.97,-1.7,2.3));
#14668=CARTESIAN_POINT('',(1.97,1.7,2.3));
#14669=CARTESIAN_POINT('',(3.07,-1.7,2.3));
#14670=CARTESIAN_POINT('',(1.97,-1.7,2.3));
#14671=CARTESIAN_POINT('',(3.07,1.7,2.3));
#14672=CARTESIAN_POINT('',(3.07,1.7,2.3));
#14673=CARTESIAN_POINT('',(1.97,1.7,2.3));
#14674=CARTESIAN_POINT('Origin',(1.97,1.7,0.46));
#14675=CARTESIAN_POINT('',(1.97,1.7,0.46));
#14676=CARTESIAN_POINT('',(1.97,1.7,0.46));
#14677=CARTESIAN_POINT('',(3.07,1.7,0.46));
#14678=CARTESIAN_POINT('',(3.07,1.7,0.46));
#14679=CARTESIAN_POINT('',(1.97,1.7,0.46));
#14680=CARTESIAN_POINT('Origin',(1.97,0.78,0.46));
#14681=CARTESIAN_POINT('',(1.97,0.78,0.46));
#14682=CARTESIAN_POINT('',(1.97,0.78,0.46));
#14683=CARTESIAN_POINT('',(3.07,0.78,0.46));
#14684=CARTESIAN_POINT('',(3.07,0.78,0.46));
#14685=CARTESIAN_POINT('',(1.97,0.78,0.46));
#14686=CARTESIAN_POINT('Origin',(1.97,0.78,1.55));
#14687=CARTESIAN_POINT('',(1.97,0.78,1.55));
#14688=CARTESIAN_POINT('',(1.97,0.78,1.55));
#14689=CARTESIAN_POINT('',(3.07,0.78,1.55));
#14690=CARTESIAN_POINT('',(3.07,0.78,1.55));
#14691=CARTESIAN_POINT('',(1.97,0.78,1.55));
#14692=CARTESIAN_POINT('Origin',(1.97,-0.78,1.55));
#14693=CARTESIAN_POINT('',(1.97,-0.78,1.55));
#14694=CARTESIAN_POINT('',(1.97,-0.78,1.55));
#14695=CARTESIAN_POINT('',(3.07,-0.78,1.55));
#14696=CARTESIAN_POINT('',(3.07,-0.78,1.55));
#14697=CARTESIAN_POINT('',(1.97,-0.78,1.55));
#14698=CARTESIAN_POINT('Origin',(1.97,-0.78,0.46));
#14699=CARTESIAN_POINT('',(1.97,-0.78,0.46));
#14700=CARTESIAN_POINT('',(1.97,-0.78,0.46));
#14701=CARTESIAN_POINT('',(3.07,-0.78,0.46));
#14702=CARTESIAN_POINT('',(3.07,-0.78,0.46));
#14703=CARTESIAN_POINT('',(1.97,-0.78,0.46));
#14704=CARTESIAN_POINT('Origin',(1.97,-1.7,0.46));
#14705=CARTESIAN_POINT('',(1.97,-1.7,0.46));
#14706=CARTESIAN_POINT('',(1.97,-1.7,0.46));
#14707=CARTESIAN_POINT('',(3.07,-1.7,0.46));
#14708=CARTESIAN_POINT('',(3.07,-1.7,0.46));
#14709=CARTESIAN_POINT('',(1.97,-1.7,0.46));
#14710=CARTESIAN_POINT('Origin',(1.97,-1.7,2.3));
#14711=CARTESIAN_POINT('',(1.97,-1.7,2.3));
#14712=CARTESIAN_POINT('',(3.07,-1.7,2.3));
#14713=CARTESIAN_POINT('Origin',(3.07,0.,1.38));
#14714=CARTESIAN_POINT('Origin',(1.97,0.,1.38));
#14715=CARTESIAN_POINT('',(0.,0.,0.));
#14716=CARTESIAN_POINT('Origin',(-1.97,-0.78,0.46));
#14717=CARTESIAN_POINT('',(-1.97,-1.7,0.46));
#14718=CARTESIAN_POINT('',(-1.97,-0.78,0.46));
#14719=CARTESIAN_POINT('',(-1.97,-1.7,0.46));
#14720=CARTESIAN_POINT('',(-3.07,-1.7,0.46));
#14721=CARTESIAN_POINT('',(-1.97,-1.7,0.46));
#14722=CARTESIAN_POINT('',(-3.07,-0.78,0.46));
#14723=CARTESIAN_POINT('',(-3.07,-1.7,0.46));
#14724=CARTESIAN_POINT('',(-1.97,-0.78,0.46));
#14725=CARTESIAN_POINT('Origin',(-1.97,-0.78,1.55));
#14726=CARTESIAN_POINT('',(-1.97,-0.78,1.55));
#14727=CARTESIAN_POINT('',(-1.97,-0.78,0.46));
#14728=CARTESIAN_POINT('',(-3.07,-0.78,1.55));
#14729=CARTESIAN_POINT('',(-3.07,-0.78,0.46));
#14730=CARTESIAN_POINT('',(-1.97,-0.78,1.55));
#14731=CARTESIAN_POINT('Origin',(-1.97,0.78,1.55));
#14732=CARTESIAN_POINT('',(-1.97,0.78,1.55));
#14733=CARTESIAN_POINT('',(-1.97,-0.78,1.55));
#14734=CARTESIAN_POINT('',(-3.07,0.78,1.55));
#14735=CARTESIAN_POINT('',(-3.07,-0.78,1.55));
#14736=CARTESIAN_POINT('',(-1.97,0.78,1.55));
#14737=CARTESIAN_POINT('Origin',(-1.97,0.78,0.46));
#14738=CARTESIAN_POINT('',(-1.97,0.78,0.46));
#14739=CARTESIAN_POINT('',(-1.97,0.78,1.55));
#14740=CARTESIAN_POINT('',(-3.07,0.78,0.46));
#14741=CARTESIAN_POINT('',(-3.07,0.78,1.55));
#14742=CARTESIAN_POINT('',(-1.97,0.78,0.46));
#14743=CARTESIAN_POINT('Origin',(-1.97,1.7,0.46));
#14744=CARTESIAN_POINT('',(-1.97,1.7,0.46));
#14745=CARTESIAN_POINT('',(-1.97,0.78,0.46));
#14746=CARTESIAN_POINT('',(-3.07,1.7,0.46));
#14747=CARTESIAN_POINT('',(-3.07,0.78,0.46));
#14748=CARTESIAN_POINT('',(-1.97,1.7,0.46));
#14749=CARTESIAN_POINT('Origin',(-1.97,1.7,2.3));
#14750=CARTESIAN_POINT('',(-1.97,1.7,2.3));
#14751=CARTESIAN_POINT('',(-1.97,1.7,0.46));
#14752=CARTESIAN_POINT('',(-3.07,1.7,2.3));
#14753=CARTESIAN_POINT('',(-3.07,1.7,0.46));
#14754=CARTESIAN_POINT('',(-1.97,1.7,2.3));
#14755=CARTESIAN_POINT('Origin',(-1.97,-1.7,2.3));
#14756=CARTESIAN_POINT('',(-1.97,-1.7,2.3));
#14757=CARTESIAN_POINT('',(-1.97,1.7,2.3));
#14758=CARTESIAN_POINT('',(-3.07,-1.7,2.3));
#14759=CARTESIAN_POINT('',(-3.07,1.7,2.3));
#14760=CARTESIAN_POINT('',(-1.97,-1.7,2.3));
#14761=CARTESIAN_POINT('Origin',(-1.97,-1.7,0.46));
#14762=CARTESIAN_POINT('',(-1.97,-1.7,2.3));
#14763=CARTESIAN_POINT('',(-3.07,-1.7,2.3));
#14764=CARTESIAN_POINT('Origin',(-1.97,0.,1.38));
#14765=CARTESIAN_POINT('Origin',(-3.07,0.,1.38));
#14766=CARTESIAN_POINT('',(0.,0.,0.));
#14767=CARTESIAN_POINT('',(0.,0.,0.));
#14768=CARTESIAN_POINT('',(0.,0.,0.));
#14769=CARTESIAN_POINT('',(0.,0.,0.));
#14770=CARTESIAN_POINT('Origin',(0.115470053837925,-0.5,-0.2));
#14771=CARTESIAN_POINT('',(0.23094010767585,-0.5,0.));
#14772=CARTESIAN_POINT('',(0.115470053837925,-0.5,-0.2));
#14773=CARTESIAN_POINT('',(0.23094010767585,-0.5,0.));
#14774=CARTESIAN_POINT('',(0.115470053837925,-0.8,-0.2));
#14775=CARTESIAN_POINT('',(0.115470053837925,-0.5,-0.2));
#14776=CARTESIAN_POINT('',(0.23094010767585,-0.8,0.));
#14777=CARTESIAN_POINT('',(0.23094010767585,-0.8,0.));
#14778=CARTESIAN_POINT('',(0.23094010767585,-0.5,0.));
#14779=CARTESIAN_POINT('Origin',(-0.115470053837925,-0.5,-0.2));
#14780=CARTESIAN_POINT('',(-0.115470053837925,-0.5,-0.2));
#14781=CARTESIAN_POINT('',(0.115470053837925,-0.5,-0.2));
#14782=CARTESIAN_POINT('',(-0.115470053837925,-0.8,-0.2));
#14783=CARTESIAN_POINT('',(-0.115470053837925,-0.5,-0.2));
#14784=CARTESIAN_POINT('',(0.115470053837925,-0.8,-0.2));
#14785=CARTESIAN_POINT('Origin',(-0.23094010767585,-0.5,-2.77555756156289E-17));
#14786=CARTESIAN_POINT('',(-0.23094010767585,-0.5,-2.82820063659975E-17));
#14787=CARTESIAN_POINT('',(-0.115470053837925,-0.5,-0.2));
#14788=CARTESIAN_POINT('',(-0.23094010767585,-0.8,-2.77555756156289E-17));
#14789=CARTESIAN_POINT('',(-0.23094010767585,-0.5,-2.82820063659975E-17));
#14790=CARTESIAN_POINT('',(-0.115470053837925,-0.8,-0.2));
#14791=CARTESIAN_POINT('Origin',(-0.115470053837925,-0.5,0.2));
#14792=CARTESIAN_POINT('',(-0.115470053837925,-0.5,0.2));
#14793=CARTESIAN_POINT('',(-0.23094010767585,-0.5,-2.82820063659975E-17));
#14794=CARTESIAN_POINT('',(-0.115470053837925,-0.8,0.2));
#14795=CARTESIAN_POINT('',(-0.115470053837925,-0.5,0.2));
#14796=CARTESIAN_POINT('',(-0.23094010767585,-0.8,-2.82820063659975E-17));
#14797=CARTESIAN_POINT('Origin',(0.115470053837925,-0.5,0.2));
#14798=CARTESIAN_POINT('',(0.115470053837925,-0.5,0.2));
#14799=CARTESIAN_POINT('',(-0.115470053837925,-0.5,0.2));
#14800=CARTESIAN_POINT('',(0.115470053837925,-0.8,0.2));
#14801=CARTESIAN_POINT('',(0.115470053837925,-0.5,0.2));
#14802=CARTESIAN_POINT('',(-0.115470053837925,-0.8,0.2));
#14803=CARTESIAN_POINT('Origin',(0.23094010767585,-0.5,0.));
#14804=CARTESIAN_POINT('',(0.115470053837925,-0.5,0.2));
#14805=CARTESIAN_POINT('',(0.115470053837925,-0.8,0.2));
#14806=CARTESIAN_POINT('Origin',(0.,-0.5,0.));
#14807=CARTESIAN_POINT('Origin',(0.,-0.8,0.));
#14808=CARTESIAN_POINT('Origin',(0.,-1.4,0.));
#14809=CARTESIAN_POINT('',(-0.24505,-1.4,3.00099698131059E-17));
#14810=CARTESIAN_POINT('Origin',(0.,-1.4,0.));
#14811=CARTESIAN_POINT('Origin',(0.375,0.5,0.));
#14812=CARTESIAN_POINT('',(-0.375,0.5,-4.59242549680257E-17));
#14813=CARTESIAN_POINT('Origin',(0.,0.5,0.));
#14814=CARTESIAN_POINT('Origin',(0.,0.475,0.));
#14815=CARTESIAN_POINT('',(-0.425,0.45,-5.20474889637625E-17));
#14816=CARTESIAN_POINT('Origin',(0.,0.45,0.));
#14817=CARTESIAN_POINT('',(-0.4,0.475,-4.89858719658941E-17));
#14818=CARTESIAN_POINT('Origin',(0.,0.24,0.));
#14819=CARTESIAN_POINT('',(-0.425,0.0299999999999998,-5.20474889637625E-17));
#14820=CARTESIAN_POINT('Origin',(0.,0.0299999999999998,0.));
#14821=CARTESIAN_POINT('',(-0.425,0.24,-5.20474889637625E-17));
#14822=CARTESIAN_POINT('Origin',(0.,0.0150000000000001,0.));
#14823=CARTESIAN_POINT('',(-0.395,4.85722573273506E-17,-4.83735485663204E-17));
#14824=CARTESIAN_POINT('Origin',(0.,0.,0.));
#14825=CARTESIAN_POINT('',(-0.41,0.0150000000000001,-5.02105187650415E-17));
#14826=CARTESIAN_POINT('Origin',(0.27,0.,0.));
#14827=CARTESIAN_POINT('',(-0.27,0.,-3.30654635769785E-17));
#14828=CARTESIAN_POINT('Origin',(0.,0.,0.));
#14829=CARTESIAN_POINT('Origin',(0.,-0.02,0.));
#14830=CARTESIAN_POINT('',(-0.24505,-0.0498999999999999,3.00099698131059E-17));
#14831=CARTESIAN_POINT('Origin',(0.,-0.0498999999999999,0.));
#14832=CARTESIAN_POINT('',(-0.26,-0.02,-3.18408167778312E-17));
#14833=CARTESIAN_POINT('Origin',(0.,-0.995,0.));
#14834=CARTESIAN_POINT('',(-0.24505,-0.995,-3.00099698131059E-17));
#14835=CARTESIAN_POINT('',(0.,0.,0.));
#14836=CARTESIAN_POINT('Origin',(0.3,0.4,0.));
#14837=CARTESIAN_POINT('',(-0.3,0.4,-3.67394039744206E-17));
#14838=CARTESIAN_POINT('Origin',(0.,0.4,0.));
#14839=CARTESIAN_POINT('Origin',(0.,0.375,0.));
#14840=CARTESIAN_POINT('',(-0.35,0.35,-4.28626379701573E-17));
#14841=CARTESIAN_POINT('Origin',(0.,0.35,0.));
#14842=CARTESIAN_POINT('',(-0.325,0.375,-3.9801020972289E-17));
#14843=CARTESIAN_POINT('Origin',(0.,0.19,0.));
#14844=CARTESIAN_POINT('',(-0.35,0.03,-4.28626379701574E-17));
#14845=CARTESIAN_POINT('Origin',(0.,0.03,0.));
#14846=CARTESIAN_POINT('',(-0.35,0.19,-4.28626379701574E-17));
#14847=CARTESIAN_POINT('Origin',(0.,0.0149999999999999,0.));
#14848=CARTESIAN_POINT('',(-0.32,-3.29597460435593E-17,-3.91886975727153E-17));
#14849=CARTESIAN_POINT('Origin',(0.,0.,0.));
#14850=CARTESIAN_POINT('',(-0.335,0.0149999999999999,-4.10256677714363E-17));
#14851=CARTESIAN_POINT('Origin',(0.22,0.,0.));
#14852=CARTESIAN_POINT('',(-0.22,-6.93889390390723E-18,-2.69422295812418E-17));
#14853=CARTESIAN_POINT('Origin',(0.,0.,0.));
#14854=CARTESIAN_POINT('Origin',(0.,-0.02,0.));
#14855=CARTESIAN_POINT('',(-0.1954,-0.0492,2.39295984553393E-17));
#14856=CARTESIAN_POINT('Origin',(0.,-0.0492,0.));
#14857=CARTESIAN_POINT('',(-0.21,-0.02,-2.57175827820944E-17));
#14858=CARTESIAN_POINT('Origin',(0.,-0.8,0.));
#14859=CARTESIAN_POINT('',(-0.1954,-1.5646,2.39295984553393E-17));
#14860=CARTESIAN_POINT('Origin',(0.,-1.5646,0.));
#14861=CARTESIAN_POINT('',(-0.1954,-0.8,-2.39295984553393E-17));
#14862=CARTESIAN_POINT('Origin',(0.,-1.58,0.));
#14863=CARTESIAN_POINT('',(-0.16,-1.6,-1.95943487863577E-17));
#14864=CARTESIAN_POINT('Origin',(0.,-1.6,0.));
#14865=CARTESIAN_POINT('',(-0.18,-1.58,-2.20436423846524E-17));
#14866=CARTESIAN_POINT('Origin',(0.,-1.6,0.));
#14867=CARTESIAN_POINT('Origin',(0.0866025403784439,-0.4,-0.15));
#14868=CARTESIAN_POINT('',(0.173205080756888,-0.4,0.));
#14869=CARTESIAN_POINT('',(0.0866025403784439,-0.4,-0.15));
#14870=CARTESIAN_POINT('',(0.173205080756888,-0.4,0.));
#14871=CARTESIAN_POINT('',(0.0866025403784439,-0.64,-0.15));
#14872=CARTESIAN_POINT('',(0.0866025403784439,-0.4,-0.15));
#14873=CARTESIAN_POINT('',(0.173205080756888,-0.64,0.));
#14874=CARTESIAN_POINT('',(0.173205080756888,-0.64,0.));
#14875=CARTESIAN_POINT('',(0.173205080756888,-0.4,0.));
#14876=CARTESIAN_POINT('Origin',(-0.0866025403784438,-0.4,-0.15));
#14877=CARTESIAN_POINT('',(-0.0866025403784438,-0.4,-0.15));
#14878=CARTESIAN_POINT('',(0.0866025403784439,-0.4,-0.15));
#14879=CARTESIAN_POINT('',(-0.0866025403784438,-0.64,-0.15));
#14880=CARTESIAN_POINT('',(-0.0866025403784438,-0.4,-0.15));
#14881=CARTESIAN_POINT('',(0.0866025403784439,-0.64,-0.15));
#14882=CARTESIAN_POINT('Origin',(-0.173205080756888,-0.4,-2.77555756156289E-17));
#14883=CARTESIAN_POINT('',(-0.173205080756888,-0.4,-2.12115047744981E-17));
#14884=CARTESIAN_POINT('',(-0.0866025403784438,-0.4,-0.15));
#14885=CARTESIAN_POINT('',(-0.173205080756888,-0.64,-2.77555756156289E-17));
#14886=CARTESIAN_POINT('',(-0.173205080756888,-0.4,-2.12115047744981E-17));
#14887=CARTESIAN_POINT('',(-0.0866025403784438,-0.64,-0.15));
#14888=CARTESIAN_POINT('Origin',(-0.0866025403784439,-0.4,0.15));
#14889=CARTESIAN_POINT('',(-0.0866025403784439,-0.4,0.15));
#14890=CARTESIAN_POINT('',(-0.173205080756888,-0.4,-2.12115047744981E-17));
#14891=CARTESIAN_POINT('',(-0.0866025403784439,-0.64,0.15));
#14892=CARTESIAN_POINT('',(-0.0866025403784439,-0.4,0.15));
#14893=CARTESIAN_POINT('',(-0.173205080756888,-0.64,-2.12115047744981E-17));
#14894=CARTESIAN_POINT('Origin',(0.0866025403784439,-0.4,0.15));
#14895=CARTESIAN_POINT('',(0.0866025403784439,-0.4,0.15));
#14896=CARTESIAN_POINT('',(-0.0866025403784439,-0.4,0.15));
#14897=CARTESIAN_POINT('',(0.0866025403784439,-0.64,0.15));
#14898=CARTESIAN_POINT('',(0.0866025403784439,-0.4,0.15));
#14899=CARTESIAN_POINT('',(-0.0866025403784439,-0.64,0.15));
#14900=CARTESIAN_POINT('Origin',(0.173205080756888,-0.4,0.));
#14901=CARTESIAN_POINT('',(0.0866025403784439,-0.4,0.15));
#14902=CARTESIAN_POINT('',(0.0866025403784439,-0.64,0.15));
#14903=CARTESIAN_POINT('Origin',(0.,-0.4,-2.77555756156289E-17));
#14904=CARTESIAN_POINT('Origin',(0.,-0.64,-2.77555756156289E-17));
#14905=CARTESIAN_POINT('',(0.,0.,0.));
#14906=CARTESIAN_POINT('',(0.,0.,0.));
#14907=CARTESIAN_POINT('',(0.,0.,0.));
#14908=CARTESIAN_POINT('',(0.,0.,0.));
#14909=CARTESIAN_POINT('',(0.,0.,0.));
#14910=CARTESIAN_POINT('',(0.,0.,0.));
#14911=CARTESIAN_POINT('',(0.,0.,0.));
#14912=CARTESIAN_POINT('',(0.,0.,0.));
#14913=CARTESIAN_POINT('',(0.,0.,0.));
#14914=CARTESIAN_POINT('',(0.,0.,0.));
#14915=CARTESIAN_POINT('',(0.,0.,0.));
#14916=CARTESIAN_POINT('',(0.,0.,0.));
#14917=CARTESIAN_POINT('',(0.,0.,0.));
#14918=CARTESIAN_POINT('',(0.,0.,0.));
#14919=CARTESIAN_POINT('',(0.,0.,0.));
#14920=CARTESIAN_POINT('',(0.,0.,0.));
#14921=CARTESIAN_POINT('',(0.,0.,0.));
#14922=CARTESIAN_POINT('',(3.,0.,0.));
#14923=CARTESIAN_POINT('',(3.,0.,-1.));
#14924=CARTESIAN_POINT('',(3.,0.,40.8));
#14925=CARTESIAN_POINT('',(2.58,0.,14.5));
#14926=CARTESIAN_POINT('',(1.2,0.,14.5));
#14927=CARTESIAN_POINT('',(1.1,0.,14.5));
#14928=CARTESIAN_POINT('',(2.58,0.,39.));
#14929=CARTESIAN_POINT('',(1.2,0.,39.));
#14930=CARTESIAN_POINT('',(1.1,0.,39.));
#14931=CARTESIAN_POINT('',(1.2,0.,16.));
#14932=CARTESIAN_POINT('',(0.23,0.,18.));
#14933=CARTESIAN_POINT('',(0.23,0.,24.));
#14934=CARTESIAN_POINT('',(0.23,0.,30.));
#14935=CARTESIAN_POINT('',(0.23,0.,36.));
#14936=CARTESIAN_POINT('',(-1.4,2.,15.55));
#14937=CARTESIAN_POINT('',(-1.4,2.,33.45));
#14938=CARTESIAN_POINT('',(3.,-3.5,1.2));
#14939=CARTESIAN_POINT('',(3.,-0.42,6.));
#14940=CARTESIAN_POINT('',(3.,-1.8,6.));
#14941=CARTESIAN_POINT('',(3.,-1.9,6.));
#14942=CARTESIAN_POINT('',(3.,3.5,1.2));
#14943=CARTESIAN_POINT('',(3.,0.42,6.));
#14944=CARTESIAN_POINT('',(3.,1.8,6.));
#14945=CARTESIAN_POINT('',(3.,1.9,6.));
#14946=CARTESIAN_POINT('',(0.,0.,0.));
#14947=CARTESIAN_POINT('',(0.,0.,0.));
#14948=CARTESIAN_POINT('',(0.,0.,0.));
#14949=CARTESIAN_POINT('',(0.,0.,0.));
#14950=CARTESIAN_POINT('',(0.,0.,0.));
#14951=CARTESIAN_POINT('',(0.,0.,0.));
#14952=CARTESIAN_POINT('',(0.,0.,0.));
#14953=CARTESIAN_POINT('',(1.2,0.,19.5));
#14954=CARTESIAN_POINT('',(-2.,-1.9,18.));
#14955=CARTESIAN_POINT('',(-2.,-1.9,21.));
#14956=CARTESIAN_POINT('',(-2.,1.9,18.));
#14957=CARTESIAN_POINT('',(-2.,1.9,21.));
#14958=CARTESIAN_POINT('',(-2.,3.,17.6));
#14959=CARTESIAN_POINT('',(0.,0.,0.));
#14960=CARTESIAN_POINT('',(-9.24327596166361E-16,-1.51929083932158E-64,
2.15435173335726));
#14961=UNCERTAINTY_MEASURE_WITH_UNIT(LENGTH_MEASURE(0.001),#15041,
'DISTANCE_ACCURACY_VALUE',
'Maximum model space distance between geometric entities at asserted c
onnectivities');
#14962=UNCERTAINTY_MEASURE_WITH_UNIT(LENGTH_MEASURE(0.001),#15041,
'DISTANCE_ACCURACY_VALUE',
'Maximum model space distance between geometric entities at asserted c
onnectivities');
#14963=UNCERTAINTY_MEASURE_WITH_UNIT(LENGTH_MEASURE(0.001),#15041,
'DISTANCE_ACCURACY_VALUE',
'Maximum model space distance between geometric entities at asserted c
onnectivities');
#14964=UNCERTAINTY_MEASURE_WITH_UNIT(LENGTH_MEASURE(0.001),#15041,
'DISTANCE_ACCURACY_VALUE',
'Maximum model space distance between geometric entities at asserted c
onnectivities');
#14965=UNCERTAINTY_MEASURE_WITH_UNIT(LENGTH_MEASURE(0.001),#15041,
'DISTANCE_ACCURACY_VALUE',
'Maximum model space distance between geometric entities at asserted c
onnectivities');
#14966=UNCERTAINTY_MEASURE_WITH_UNIT(LENGTH_MEASURE(0.001),#15041,
'DISTANCE_ACCURACY_VALUE',
'Maximum model space distance between geometric entities at asserted c
onnectivities');
#14967=UNCERTAINTY_MEASURE_WITH_UNIT(LENGTH_MEASURE(0.001),#15041,
'DISTANCE_ACCURACY_VALUE',
'Maximum model space distance between geometric entities at asserted c
onnectivities');
#14968=UNCERTAINTY_MEASURE_WITH_UNIT(LENGTH_MEASURE(0.001),#15041,
'DISTANCE_ACCURACY_VALUE',
'Maximum model space distance between geometric entities at asserted c
onnectivities');
#14969=UNCERTAINTY_MEASURE_WITH_UNIT(LENGTH_MEASURE(0.001),#15041,
'DISTANCE_ACCURACY_VALUE',
'Maximum model space distance between geometric entities at asserted c
onnectivities');
#14970=UNCERTAINTY_MEASURE_WITH_UNIT(LENGTH_MEASURE(0.001),#15041,
'DISTANCE_ACCURACY_VALUE',
'Maximum model space distance between geometric entities at asserted c
onnectivities');
#14971=UNCERTAINTY_MEASURE_WITH_UNIT(LENGTH_MEASURE(0.001),#15041,
'DISTANCE_ACCURACY_VALUE',
'Maximum model space distance between geometric entities at asserted c
onnectivities');
#14972=UNCERTAINTY_MEASURE_WITH_UNIT(LENGTH_MEASURE(0.001),#15041,
'DISTANCE_ACCURACY_VALUE',
'Maximum model space distance between geometric entities at asserted c
onnectivities');
#14973=UNCERTAINTY_MEASURE_WITH_UNIT(LENGTH_MEASURE(0.001),#15041,
'DISTANCE_ACCURACY_VALUE',
'Maximum model space distance between geometric entities at asserted c
onnectivities');
#14974=UNCERTAINTY_MEASURE_WITH_UNIT(LENGTH_MEASURE(0.001),#15041,
'DISTANCE_ACCURACY_VALUE',
'Maximum model space distance between geometric entities at asserted c
onnectivities');
#14975=UNCERTAINTY_MEASURE_WITH_UNIT(LENGTH_MEASURE(0.001),#15041,
'DISTANCE_ACCURACY_VALUE',
'Maximum model space distance between geometric entities at asserted c
onnectivities');
#14976=UNCERTAINTY_MEASURE_WITH_UNIT(LENGTH_MEASURE(0.001),#15041,
'DISTANCE_ACCURACY_VALUE',
'Maximum model space distance between geometric entities at asserted c
onnectivities');
#14977=UNCERTAINTY_MEASURE_WITH_UNIT(LENGTH_MEASURE(0.001),#15041,
'DISTANCE_ACCURACY_VALUE',
'Maximum model space distance between geometric entities at asserted c
onnectivities');
#14978=UNCERTAINTY_MEASURE_WITH_UNIT(LENGTH_MEASURE(0.001),#15041,
'DISTANCE_ACCURACY_VALUE',
'Maximum model space distance between geometric entities at asserted c
onnectivities');
#14979=UNCERTAINTY_MEASURE_WITH_UNIT(LENGTH_MEASURE(0.001),#15041,
'DISTANCE_ACCURACY_VALUE',
'Maximum model space distance between geometric entities at asserted c
onnectivities');
#14980=UNCERTAINTY_MEASURE_WITH_UNIT(LENGTH_MEASURE(0.001),#15041,
'DISTANCE_ACCURACY_VALUE',
'Maximum model space distance between geometric entities at asserted c
onnectivities');
#14981=UNCERTAINTY_MEASURE_WITH_UNIT(LENGTH_MEASURE(0.001),#15041,
'DISTANCE_ACCURACY_VALUE',
'Maximum model space distance between geometric entities at asserted c
onnectivities');
#14982=UNCERTAINTY_MEASURE_WITH_UNIT(LENGTH_MEASURE(0.001),#15041,
'DISTANCE_ACCURACY_VALUE',
'Maximum model space distance between geometric entities at asserted c
onnectivities');
#14983=UNCERTAINTY_MEASURE_WITH_UNIT(LENGTH_MEASURE(0.001),#15041,
'DISTANCE_ACCURACY_VALUE',
'Maximum model space distance between geometric entities at asserted c
onnectivities');
#14984=UNCERTAINTY_MEASURE_WITH_UNIT(LENGTH_MEASURE(0.001),#15041,
'DISTANCE_ACCURACY_VALUE',
'Maximum model space distance between geometric entities at asserted c
onnectivities');
#14985=UNCERTAINTY_MEASURE_WITH_UNIT(LENGTH_MEASURE(0.001),#15041,
'DISTANCE_ACCURACY_VALUE',
'Maximum model space distance between geometric entities at asserted c
onnectivities');
#14986=UNCERTAINTY_MEASURE_WITH_UNIT(LENGTH_MEASURE(0.001),#15041,
'DISTANCE_ACCURACY_VALUE',
'Maximum model space distance between geometric entities at asserted c
onnectivities');
#14987=UNCERTAINTY_MEASURE_WITH_UNIT(LENGTH_MEASURE(0.001),#15041,
'DISTANCE_ACCURACY_VALUE',
'Maximum model space distance between geometric entities at asserted c
onnectivities');
#14988=UNCERTAINTY_MEASURE_WITH_UNIT(LENGTH_MEASURE(0.001),#15041,
'DISTANCE_ACCURACY_VALUE',
'Maximum model space distance between geometric entities at asserted c
onnectivities');
#14989=UNCERTAINTY_MEASURE_WITH_UNIT(LENGTH_MEASURE(0.001),#15041,
'DISTANCE_ACCURACY_VALUE',
'Maximum model space distance between geometric entities at asserted c
onnectivities');
#14990=UNCERTAINTY_MEASURE_WITH_UNIT(LENGTH_MEASURE(0.001),#15041,
'DISTANCE_ACCURACY_VALUE',
'Maximum model space distance between geometric entities at asserted c
onnectivities');
#14991=UNCERTAINTY_MEASURE_WITH_UNIT(LENGTH_MEASURE(0.001),#15041,
'DISTANCE_ACCURACY_VALUE',
'Maximum model space distance between geometric entities at asserted c
onnectivities');
#14992=UNCERTAINTY_MEASURE_WITH_UNIT(LENGTH_MEASURE(0.001),#15041,
'DISTANCE_ACCURACY_VALUE',
'Maximum model space distance between geometric entities at asserted c
onnectivities');
#14993=UNCERTAINTY_MEASURE_WITH_UNIT(LENGTH_MEASURE(0.001),#15041,
'DISTANCE_ACCURACY_VALUE',
'Maximum model space distance between geometric entities at asserted c
onnectivities');
#14994=UNCERTAINTY_MEASURE_WITH_UNIT(LENGTH_MEASURE(0.001),#15041,
'DISTANCE_ACCURACY_VALUE',
'Maximum model space distance between geometric entities at asserted c
onnectivities');
#14995=UNCERTAINTY_MEASURE_WITH_UNIT(LENGTH_MEASURE(0.001),#15041,
'DISTANCE_ACCURACY_VALUE',
'Maximum model space distance between geometric entities at asserted c
onnectivities');
#14996=UNCERTAINTY_MEASURE_WITH_UNIT(LENGTH_MEASURE(0.001),#15041,
'DISTANCE_ACCURACY_VALUE',
'Maximum model space distance between geometric entities at asserted c
onnectivities');
#14997=UNCERTAINTY_MEASURE_WITH_UNIT(LENGTH_MEASURE(0.001),#15041,
'DISTANCE_ACCURACY_VALUE',
'Maximum model space distance between geometric entities at asserted c
onnectivities');
#14998=UNCERTAINTY_MEASURE_WITH_UNIT(LENGTH_MEASURE(0.001),#15041,
'DISTANCE_ACCURACY_VALUE',
'Maximum model space distance between geometric entities at asserted c
onnectivities');
#14999=UNCERTAINTY_MEASURE_WITH_UNIT(LENGTH_MEASURE(0.001),#15041,
'DISTANCE_ACCURACY_VALUE',
'Maximum model space distance between geometric entities at asserted c
onnectivities');
#15000=UNCERTAINTY_MEASURE_WITH_UNIT(LENGTH_MEASURE(0.001),#15041,
'DISTANCE_ACCURACY_VALUE',
'Maximum model space distance between geometric entities at asserted c
onnectivities');
#15001=(
GEOMETRIC_REPRESENTATION_CONTEXT(3)
GLOBAL_UNCERTAINTY_ASSIGNED_CONTEXT((#14961))
GLOBAL_UNIT_ASSIGNED_CONTEXT((#15041,#15043,#15044))
REPRESENTATION_CONTEXT('','3D')
);
#15002=(
GEOMETRIC_REPRESENTATION_CONTEXT(3)
GLOBAL_UNCERTAINTY_ASSIGNED_CONTEXT((#14962))
GLOBAL_UNIT_ASSIGNED_CONTEXT((#15041,#15043,#15044))
REPRESENTATION_CONTEXT('','3D')
);
#15003=(
GEOMETRIC_REPRESENTATION_CONTEXT(3)
GLOBAL_UNCERTAINTY_ASSIGNED_CONTEXT((#14963))
GLOBAL_UNIT_ASSIGNED_CONTEXT((#15041,#15043,#15044))
REPRESENTATION_CONTEXT('','3D')
);
#15004=(
GEOMETRIC_REPRESENTATION_CONTEXT(3)
GLOBAL_UNCERTAINTY_ASSIGNED_CONTEXT((#14964))
GLOBAL_UNIT_ASSIGNED_CONTEXT((#15041,#15043,#15044))
REPRESENTATION_CONTEXT('','3D')
);
#15005=(
GEOMETRIC_REPRESENTATION_CONTEXT(3)
GLOBAL_UNCERTAINTY_ASSIGNED_CONTEXT((#14965))
GLOBAL_UNIT_ASSIGNED_CONTEXT((#15041,#15043,#15044))
REPRESENTATION_CONTEXT('','3D')
);
#15006=(
GEOMETRIC_REPRESENTATION_CONTEXT(3)
GLOBAL_UNCERTAINTY_ASSIGNED_CONTEXT((#14966))
GLOBAL_UNIT_ASSIGNED_CONTEXT((#15041,#15043,#15044))
REPRESENTATION_CONTEXT('','3D')
);
#15007=(
GEOMETRIC_REPRESENTATION_CONTEXT(3)
GLOBAL_UNCERTAINTY_ASSIGNED_CONTEXT((#14967))
GLOBAL_UNIT_ASSIGNED_CONTEXT((#15041,#15043,#15044))
REPRESENTATION_CONTEXT('','3D')
);
#15008=(
GEOMETRIC_REPRESENTATION_CONTEXT(3)
GLOBAL_UNCERTAINTY_ASSIGNED_CONTEXT((#14968))
GLOBAL_UNIT_ASSIGNED_CONTEXT((#15041,#15043,#15044))
REPRESENTATION_CONTEXT('','3D')
);
#15009=(
GEOMETRIC_REPRESENTATION_CONTEXT(3)
GLOBAL_UNCERTAINTY_ASSIGNED_CONTEXT((#14969))
GLOBAL_UNIT_ASSIGNED_CONTEXT((#15041,#15043,#15044))
REPRESENTATION_CONTEXT('','3D')
);
#15010=(
GEOMETRIC_REPRESENTATION_CONTEXT(3)
GLOBAL_UNCERTAINTY_ASSIGNED_CONTEXT((#14970))
GLOBAL_UNIT_ASSIGNED_CONTEXT((#15041,#15043,#15044))
REPRESENTATION_CONTEXT('','3D')
);
#15011=(
GEOMETRIC_REPRESENTATION_CONTEXT(3)
GLOBAL_UNCERTAINTY_ASSIGNED_CONTEXT((#14971))
GLOBAL_UNIT_ASSIGNED_CONTEXT((#15041,#15043,#15044))
REPRESENTATION_CONTEXT('','3D')
);
#15012=(
GEOMETRIC_REPRESENTATION_CONTEXT(3)
GLOBAL_UNCERTAINTY_ASSIGNED_CONTEXT((#14972))
GLOBAL_UNIT_ASSIGNED_CONTEXT((#15041,#15043,#15044))
REPRESENTATION_CONTEXT('','3D')
);
#15013=(
GEOMETRIC_REPRESENTATION_CONTEXT(3)
GLOBAL_UNCERTAINTY_ASSIGNED_CONTEXT((#14973))
GLOBAL_UNIT_ASSIGNED_CONTEXT((#15041,#15043,#15044))
REPRESENTATION_CONTEXT('','3D')
);
#15014=(
GEOMETRIC_REPRESENTATION_CONTEXT(3)
GLOBAL_UNCERTAINTY_ASSIGNED_CONTEXT((#14974))
GLOBAL_UNIT_ASSIGNED_CONTEXT((#15041,#15043,#15044))
REPRESENTATION_CONTEXT('','3D')
);
#15015=(
GEOMETRIC_REPRESENTATION_CONTEXT(3)
GLOBAL_UNCERTAINTY_ASSIGNED_CONTEXT((#14975))
GLOBAL_UNIT_ASSIGNED_CONTEXT((#15041,#15043,#15044))
REPRESENTATION_CONTEXT('','3D')
);
#15016=(
GEOMETRIC_REPRESENTATION_CONTEXT(3)
GLOBAL_UNCERTAINTY_ASSIGNED_CONTEXT((#14976))
GLOBAL_UNIT_ASSIGNED_CONTEXT((#15041,#15043,#15044))
REPRESENTATION_CONTEXT('','3D')
);
#15017=(
GEOMETRIC_REPRESENTATION_CONTEXT(3)
GLOBAL_UNCERTAINTY_ASSIGNED_CONTEXT((#14977))
GLOBAL_UNIT_ASSIGNED_CONTEXT((#15041,#15043,#15044))
REPRESENTATION_CONTEXT('','3D')
);
#15018=(
GEOMETRIC_REPRESENTATION_CONTEXT(3)
GLOBAL_UNCERTAINTY_ASSIGNED_CONTEXT((#14978))
GLOBAL_UNIT_ASSIGNED_CONTEXT((#15041,#15043,#15044))
REPRESENTATION_CONTEXT('','3D')
);
#15019=(
GEOMETRIC_REPRESENTATION_CONTEXT(3)
GLOBAL_UNCERTAINTY_ASSIGNED_CONTEXT((#14979))
GLOBAL_UNIT_ASSIGNED_CONTEXT((#15041,#15043,#15044))
REPRESENTATION_CONTEXT('','3D')
);
#15020=(
GEOMETRIC_REPRESENTATION_CONTEXT(3)
GLOBAL_UNCERTAINTY_ASSIGNED_CONTEXT((#14980))
GLOBAL_UNIT_ASSIGNED_CONTEXT((#15041,#15043,#15044))
REPRESENTATION_CONTEXT('','3D')
);
#15021=(
GEOMETRIC_REPRESENTATION_CONTEXT(3)
GLOBAL_UNCERTAINTY_ASSIGNED_CONTEXT((#14981))
GLOBAL_UNIT_ASSIGNED_CONTEXT((#15041,#15043,#15044))
REPRESENTATION_CONTEXT('','3D')
);
#15022=(
GEOMETRIC_REPRESENTATION_CONTEXT(3)
GLOBAL_UNCERTAINTY_ASSIGNED_CONTEXT((#14982))
GLOBAL_UNIT_ASSIGNED_CONTEXT((#15041,#15043,#15044))
REPRESENTATION_CONTEXT('','3D')
);
#15023=(
GEOMETRIC_REPRESENTATION_CONTEXT(3)
GLOBAL_UNCERTAINTY_ASSIGNED_CONTEXT((#14983))
GLOBAL_UNIT_ASSIGNED_CONTEXT((#15041,#15043,#15044))
REPRESENTATION_CONTEXT('','3D')
);
#15024=(
GEOMETRIC_REPRESENTATION_CONTEXT(3)
GLOBAL_UNCERTAINTY_ASSIGNED_CONTEXT((#14984))
GLOBAL_UNIT_ASSIGNED_CONTEXT((#15041,#15043,#15044))
REPRESENTATION_CONTEXT('','3D')
);
#15025=(
GEOMETRIC_REPRESENTATION_CONTEXT(3)
GLOBAL_UNCERTAINTY_ASSIGNED_CONTEXT((#14985))
GLOBAL_UNIT_ASSIGNED_CONTEXT((#15041,#15043,#15044))
REPRESENTATION_CONTEXT('','3D')
);
#15026=(
GEOMETRIC_REPRESENTATION_CONTEXT(3)
GLOBAL_UNCERTAINTY_ASSIGNED_CONTEXT((#14986))
GLOBAL_UNIT_ASSIGNED_CONTEXT((#15041,#15043,#15044))
REPRESENTATION_CONTEXT('','3D')
);
#15027=(
GEOMETRIC_REPRESENTATION_CONTEXT(3)
GLOBAL_UNCERTAINTY_ASSIGNED_CONTEXT((#14987))
GLOBAL_UNIT_ASSIGNED_CONTEXT((#15041,#15043,#15044))
REPRESENTATION_CONTEXT('','3D')
);
#15028=(
GEOMETRIC_REPRESENTATION_CONTEXT(3)
GLOBAL_UNCERTAINTY_ASSIGNED_CONTEXT((#14988))
GLOBAL_UNIT_ASSIGNED_CONTEXT((#15041,#15043,#15044))
REPRESENTATION_CONTEXT('','3D')
);
#15029=(
GEOMETRIC_REPRESENTATION_CONTEXT(3)
GLOBAL_UNCERTAINTY_ASSIGNED_CONTEXT((#14989))
GLOBAL_UNIT_ASSIGNED_CONTEXT((#15041,#15043,#15044))
REPRESENTATION_CONTEXT('','3D')
);
#15030=(
GEOMETRIC_REPRESENTATION_CONTEXT(3)
GLOBAL_UNCERTAINTY_ASSIGNED_CONTEXT((#14990))
GLOBAL_UNIT_ASSIGNED_CONTEXT((#15041,#15043,#15044))
REPRESENTATION_CONTEXT('','3D')
);
#15031=(
GEOMETRIC_REPRESENTATION_CONTEXT(3)
GLOBAL_UNCERTAINTY_ASSIGNED_CONTEXT((#14991))
GLOBAL_UNIT_ASSIGNED_CONTEXT((#15041,#15043,#15044))
REPRESENTATION_CONTEXT('','3D')
);
#15032=(
GEOMETRIC_REPRESENTATION_CONTEXT(3)
GLOBAL_UNCERTAINTY_ASSIGNED_CONTEXT((#14992))
GLOBAL_UNIT_ASSIGNED_CONTEXT((#15041,#15043,#15044))
REPRESENTATION_CONTEXT('','3D')
);
#15033=(
GEOMETRIC_REPRESENTATION_CONTEXT(3)
GLOBAL_UNCERTAINTY_ASSIGNED_CONTEXT((#14993))
GLOBAL_UNIT_ASSIGNED_CONTEXT((#15041,#15043,#15044))
REPRESENTATION_CONTEXT('','3D')
);
#15034=(
GEOMETRIC_REPRESENTATION_CONTEXT(3)
GLOBAL_UNCERTAINTY_ASSIGNED_CONTEXT((#14994))
GLOBAL_UNIT_ASSIGNED_CONTEXT((#15041,#15043,#15044))
REPRESENTATION_CONTEXT('','3D')
);
#15035=(
GEOMETRIC_REPRESENTATION_CONTEXT(3)
GLOBAL_UNCERTAINTY_ASSIGNED_CONTEXT((#14995))
GLOBAL_UNIT_ASSIGNED_CONTEXT((#15041,#15043,#15044))
REPRESENTATION_CONTEXT('','3D')
);
#15036=(
GEOMETRIC_REPRESENTATION_CONTEXT(3)
GLOBAL_UNCERTAINTY_ASSIGNED_CONTEXT((#14996))
GLOBAL_UNIT_ASSIGNED_CONTEXT((#15041,#15043,#15044))
REPRESENTATION_CONTEXT('','3D')
);
#15037=(
GEOMETRIC_REPRESENTATION_CONTEXT(3)
GLOBAL_UNCERTAINTY_ASSIGNED_CONTEXT((#14997))
GLOBAL_UNIT_ASSIGNED_CONTEXT((#15041,#15043,#15044))
REPRESENTATION_CONTEXT('','3D')
);
#15038=(
GEOMETRIC_REPRESENTATION_CONTEXT(3)
GLOBAL_UNCERTAINTY_ASSIGNED_CONTEXT((#14998))
GLOBAL_UNIT_ASSIGNED_CONTEXT((#15041,#15043,#15044))
REPRESENTATION_CONTEXT('','3D')
);
#15039=(
GEOMETRIC_REPRESENTATION_CONTEXT(3)
GLOBAL_UNCERTAINTY_ASSIGNED_CONTEXT((#14999))
GLOBAL_UNIT_ASSIGNED_CONTEXT((#15041,#15043,#15044))
REPRESENTATION_CONTEXT('','3D')
);
#15040=(
GEOMETRIC_REPRESENTATION_CONTEXT(3)
GLOBAL_UNCERTAINTY_ASSIGNED_CONTEXT((#15000))
GLOBAL_UNIT_ASSIGNED_CONTEXT((#15041,#15043,#15044))
REPRESENTATION_CONTEXT('','3D')
);
#15041=(
LENGTH_UNIT()
NAMED_UNIT(*)
SI_UNIT(.CENTI.,.METRE.)
);
#15042=(
LENGTH_UNIT()
NAMED_UNIT(*)
SI_UNIT($,.METRE.)
);
#15043=(
NAMED_UNIT(*)
PLANE_ANGLE_UNIT()
SI_UNIT($,.RADIAN.)
);
#15044=(
NAMED_UNIT(*)
SI_UNIT($,.STERADIAN.)
SOLID_ANGLE_UNIT()
);
#15045=SHAPE_DEFINITION_REPRESENTATION(#15084,#15182);
#15046=SHAPE_DEFINITION_REPRESENTATION(#15085,#15183);
#15047=SHAPE_DEFINITION_REPRESENTATION(#15086,#15184);
#15048=SHAPE_DEFINITION_REPRESENTATION(#15087,#15185);
#15049=SHAPE_DEFINITION_REPRESENTATION(#15088,#15186);
#15050=SHAPE_DEFINITION_REPRESENTATION(#15089,#15187);
#15051=SHAPE_DEFINITION_REPRESENTATION(#15090,#15188);
#15052=SHAPE_DEFINITION_REPRESENTATION(#15091,#15189);
#15053=SHAPE_DEFINITION_REPRESENTATION(#15092,#15190);
#15054=SHAPE_DEFINITION_REPRESENTATION(#15093,#15191);
#15055=SHAPE_DEFINITION_REPRESENTATION(#15094,#15192);
#15056=SHAPE_DEFINITION_REPRESENTATION(#15095,#15193);
#15057=SHAPE_DEFINITION_REPRESENTATION(#15096,#15194);
#15058=SHAPE_DEFINITION_REPRESENTATION(#15097,#15195);
#15059=SHAPE_DEFINITION_REPRESENTATION(#15098,#15196);
#15060=SHAPE_DEFINITION_REPRESENTATION(#15099,#15197);
#15061=SHAPE_DEFINITION_REPRESENTATION(#15100,#15198);
#15062=SHAPE_DEFINITION_REPRESENTATION(#15101,#15199);
#15063=SHAPE_DEFINITION_REPRESENTATION(#15102,#15200);
#15064=SHAPE_DEFINITION_REPRESENTATION(#15103,#15201);
#15065=SHAPE_DEFINITION_REPRESENTATION(#15104,#15202);
#15066=SHAPE_DEFINITION_REPRESENTATION(#15105,#15203);
#15067=SHAPE_DEFINITION_REPRESENTATION(#15106,#15204);
#15068=SHAPE_DEFINITION_REPRESENTATION(#15107,#15205);
#15069=SHAPE_DEFINITION_REPRESENTATION(#15108,#15206);
#15070=SHAPE_DEFINITION_REPRESENTATION(#15109,#15207);
#15071=SHAPE_DEFINITION_REPRESENTATION(#15110,#15208);
#15072=SHAPE_DEFINITION_REPRESENTATION(#15111,#15209);
#15073=SHAPE_DEFINITION_REPRESENTATION(#15112,#15210);
#15074=SHAPE_DEFINITION_REPRESENTATION(#15113,#15211);
#15075=SHAPE_DEFINITION_REPRESENTATION(#15114,#15212);
#15076=SHAPE_DEFINITION_REPRESENTATION(#15115,#15213);
#15077=SHAPE_DEFINITION_REPRESENTATION(#15116,#15214);
#15078=SHAPE_DEFINITION_REPRESENTATION(#15117,#15215);
#15079=SHAPE_DEFINITION_REPRESENTATION(#15118,#15216);
#15080=SHAPE_DEFINITION_REPRESENTATION(#15119,#15217);
#15081=SHAPE_DEFINITION_REPRESENTATION(#15120,#15218);
#15082=SHAPE_DEFINITION_REPRESENTATION(#15124,#15219);
#15083=SHAPE_DEFINITION_REPRESENTATION(#15125,#15220);
#15084=PRODUCT_DEFINITION_SHAPE('',$,#15222);
#15085=PRODUCT_DEFINITION_SHAPE('',$,#15223);
#15086=PRODUCT_DEFINITION_SHAPE('',$,#15224);
#15087=PRODUCT_DEFINITION_SHAPE('',$,#15225);
#15088=PRODUCT_DEFINITION_SHAPE('',$,#15226);
#15089=PRODUCT_DEFINITION_SHAPE('',$,#15227);
#15090=PRODUCT_DEFINITION_SHAPE('',$,#15228);
#15091=PRODUCT_DEFINITION_SHAPE('',$,#15229);
#15092=PRODUCT_DEFINITION_SHAPE('',$,#15230);
#15093=PRODUCT_DEFINITION_SHAPE('',$,#15231);
#15094=PRODUCT_DEFINITION_SHAPE('',$,#15232);
#15095=PRODUCT_DEFINITION_SHAPE('',$,#15233);
#15096=PRODUCT_DEFINITION_SHAPE('',$,#15234);
#15097=PRODUCT_DEFINITION_SHAPE('',$,#15235);
#15098=PRODUCT_DEFINITION_SHAPE('',$,#15236);
#15099=PRODUCT_DEFINITION_SHAPE('',$,#15237);
#15100=PRODUCT_DEFINITION_SHAPE('',$,#15238);
#15101=PRODUCT_DEFINITION_SHAPE('',$,#15239);
#15102=PRODUCT_DEFINITION_SHAPE('',$,#15240);
#15103=PRODUCT_DEFINITION_SHAPE('',$,#15241);
#15104=PRODUCT_DEFINITION_SHAPE('',$,#15242);
#15105=PRODUCT_DEFINITION_SHAPE('',$,#15243);
#15106=PRODUCT_DEFINITION_SHAPE('',$,#15244);
#15107=PRODUCT_DEFINITION_SHAPE('',$,#15245);
#15108=PRODUCT_DEFINITION_SHAPE('',$,#15246);
#15109=PRODUCT_DEFINITION_SHAPE('',$,#15247);
#15110=PRODUCT_DEFINITION_SHAPE('',$,#15248);
#15111=PRODUCT_DEFINITION_SHAPE('',$,#15249);
#15112=PRODUCT_DEFINITION_SHAPE('',$,#15250);
#15113=PRODUCT_DEFINITION_SHAPE('',$,#15251);
#15114=PRODUCT_DEFINITION_SHAPE('',$,#15252);
#15115=PRODUCT_DEFINITION_SHAPE('',$,#15253);
#15116=PRODUCT_DEFINITION_SHAPE('',$,#15254);
#15117=PRODUCT_DEFINITION_SHAPE('',$,#15255);
#15118=PRODUCT_DEFINITION_SHAPE('',$,#15256);
#15119=PRODUCT_DEFINITION_SHAPE('',$,#15257);
#15120=PRODUCT_DEFINITION_SHAPE('',$,#15258);
#15121=PRODUCT_DEFINITION_SHAPE($,$,#188);
#15122=PRODUCT_DEFINITION_SHAPE($,$,#189);
#15123=PRODUCT_DEFINITION_SHAPE($,$,#190);
#15124=PRODUCT_DEFINITION_SHAPE('',$,#15259);
#15125=PRODUCT_DEFINITION_SHAPE('',$,#15260);
#15126=PRODUCT_DEFINITION_SHAPE($,$,#191);
#15127=PRODUCT_DEFINITION_SHAPE($,$,#192);
#15128=PRODUCT_DEFINITION_SHAPE($,$,#193);
#15129=PRODUCT_DEFINITION_SHAPE($,$,#194);
#15130=PRODUCT_DEFINITION_SHAPE($,$,#195);
#15131=PRODUCT_DEFINITION_SHAPE($,$,#196);
#15132=PRODUCT_DEFINITION_SHAPE($,$,#197);
#15133=PRODUCT_DEFINITION_SHAPE($,$,#198);
#15134=PRODUCT_DEFINITION_SHAPE($,$,#199);
#15135=PRODUCT_DEFINITION_SHAPE($,$,#200);
#15136=PRODUCT_DEFINITION_SHAPE($,$,#201);
#15137=PRODUCT_DEFINITION_SHAPE($,$,#202);
#15138=PRODUCT_DEFINITION_SHAPE($,$,#203);
#15139=PRODUCT_DEFINITION_SHAPE($,$,#204);
#15140=PRODUCT_DEFINITION_SHAPE($,$,#205);
#15141=PRODUCT_DEFINITION_SHAPE($,$,#206);
#15142=PRODUCT_DEFINITION_SHAPE($,$,#207);
#15143=PRODUCT_DEFINITION_SHAPE($,$,#208);
#15144=PRODUCT_DEFINITION_SHAPE($,$,#209);
#15145=PRODUCT_DEFINITION_SHAPE($,$,#210);
#15146=PRODUCT_DEFINITION_SHAPE($,$,#211);
#15147=PRODUCT_DEFINITION_SHAPE($,$,#212);
#15148=PRODUCT_DEFINITION_SHAPE($,$,#213);
#15149=PRODUCT_DEFINITION_SHAPE($,$,#214);
#15150=PRODUCT_DEFINITION_SHAPE($,$,#215);
#15151=PRODUCT_DEFINITION_SHAPE($,$,#216);
#15152=PRODUCT_DEFINITION_SHAPE($,$,#217);
#15153=PRODUCT_DEFINITION_SHAPE($,$,#218);
#15154=PRODUCT_DEFINITION_SHAPE($,$,#219);
#15155=PRODUCT_DEFINITION_SHAPE($,$,#220);
#15156=PRODUCT_DEFINITION_SHAPE($,$,#221);
#15157=PRODUCT_DEFINITION_SHAPE($,$,#222);
#15158=PRODUCT_DEFINITION_SHAPE($,$,#223);
#15159=PRODUCT_DEFINITION_SHAPE($,$,#224);
#15160=PRODUCT_DEFINITION_SHAPE($,$,#225);
#15161=PRODUCT_DEFINITION_SHAPE($,$,#226);
#15162=PRODUCT_DEFINITION_SHAPE($,$,#227);
#15163=PRODUCT_DEFINITION_SHAPE($,$,#228);
#15164=PRODUCT_DEFINITION_SHAPE($,$,#229);
#15165=PRODUCT_DEFINITION_SHAPE($,$,#230);
#15166=PRODUCT_DEFINITION_SHAPE($,$,#231);
#15167=PRODUCT_DEFINITION_SHAPE($,$,#232);
#15168=PRODUCT_DEFINITION_SHAPE($,$,#233);
#15169=PRODUCT_DEFINITION_SHAPE($,$,#234);
#15170=PRODUCT_DEFINITION_SHAPE($,$,#235);
#15171=PRODUCT_DEFINITION_SHAPE($,$,#236);
#15172=PRODUCT_DEFINITION_SHAPE($,$,#237);
#15173=PRODUCT_DEFINITION_SHAPE($,$,#238);
#15174=PRODUCT_DEFINITION_SHAPE($,$,#239);
#15175=PRODUCT_DEFINITION_SHAPE($,$,#240);
#15176=PRODUCT_DEFINITION_SHAPE($,$,#241);
#15177=PRODUCT_DEFINITION_SHAPE($,$,#242);
#15178=PRODUCT_DEFINITION_SHAPE($,$,#243);
#15179=PRODUCT_DEFINITION_SHAPE($,$,#244);
#15180=PRODUCT_DEFINITION_SHAPE($,$,#245);
#15181=PRODUCT_DEFINITION_SHAPE($,$,#246);
#15182=SHAPE_REPRESENTATION('',(#7498,#8219,#8220),#15001);
#15183=SHAPE_REPRESENTATION('',(#7499,#8165,#8166,#8167,#8168,#8169,#8170,
#8171,#8172,#8173,#8174,#8175,#8176,#8177,#8178,#8179,#8180,#8181,#8182,
#8183,#8184,#8185,#8186,#8187,#8188,#8189,#8190,#8191,#8192,#8193,#8194,
#8195,#8196,#8197,#8198,#8199,#8200,#8201,#8202,#8203,#8204,#8205),#15002);
#15184=SHAPE_REPRESENTATION('',(#7500),#15003);
#15185=SHAPE_REPRESENTATION('',(#7526),#15004);
#15186=SHAPE_REPRESENTATION('',(#7533),#15005);
#15187=SHAPE_REPRESENTATION('',(#7540),#15006);
#15188=SHAPE_REPRESENTATION('',(#7550),#15007);
#15189=SHAPE_REPRESENTATION('',(#7585),#15008);
#15190=SHAPE_REPRESENTATION('',(#7595),#15009);
#15191=SHAPE_REPRESENTATION('',(#7605),#15010);
#15192=SHAPE_REPRESENTATION('',(#7625),#15011);
#15193=SHAPE_REPRESENTATION('',(#7634),#15012);
#15194=SHAPE_REPRESENTATION('',(#7657),#15013);
#15195=SHAPE_REPRESENTATION('',(#7671),#15014);
#15196=SHAPE_REPRESENTATION('',(#7680),#15015);
#15197=SHAPE_REPRESENTATION('',(#7694),#15016);
#15198=SHAPE_REPRESENTATION('',(#7703),#15017);
#15199=SHAPE_REPRESENTATION('',(#7708),#15018);
#15200=SHAPE_REPRESENTATION('',(#7730),#15019);
#15201=SHAPE_REPRESENTATION('',(#7752),#15020);
#15202=SHAPE_REPRESENTATION('',(#7802),#15021);
#15203=SHAPE_REPRESENTATION('',(#7845),#15022);
#15204=SHAPE_REPRESENTATION('',(#7873),#15023);
#15205=SHAPE_REPRESENTATION('',(#7899),#15024);
#15206=SHAPE_REPRESENTATION('',(#7920),#15025);
#15207=SHAPE_REPRESENTATION('',(#7931,#8206,#8207,#8208,#8209,#8210,#8211,
#8212,#8213,#8214,#8215,#8216,#8217,#8218),#15026);
#15208=SHAPE_REPRESENTATION('',(#7932),#15027);
#15209=SHAPE_REPRESENTATION('',(#7983),#15028);
#15210=SHAPE_REPRESENTATION('',(#7992),#15029);
#15211=SHAPE_REPRESENTATION('',(#8010),#15030);
#15212=SHAPE_REPRESENTATION('',(#8019),#15031);
#15213=SHAPE_REPRESENTATION('',(#8033),#15032);
#15214=SHAPE_REPRESENTATION('',(#8040),#15033);
#15215=SHAPE_REPRESENTATION('',(#8050,#8112,#8113,#8114),#15034);
#15216=SHAPE_REPRESENTATION('',(#8051),#15035);
#15217=SHAPE_REPRESENTATION('',(#8090),#15036);
#15218=SHAPE_REPRESENTATION('',(#8101),#15037);
#15219=SHAPE_REPRESENTATION('',(#8115),#15038);
#15220=SHAPE_REPRESENTATION('',(#8139),#15039);
#15221=PRODUCT_DEFINITION_CONTEXT('part definition',#15340,'design');
#15222=PRODUCT_DEFINITION('PAT-117',
'PAT-117',#15261,#15221);
#15223=PRODUCT_DEFINITION('Column and spring barrel',
'Column and spring barrel',#15262,#15221);
#15224=PRODUCT_DEFINITION('Base foot','Base foot',#15263,#15221);
#15225=PRODUCT_DEFINITION('Foot strip','Foot strip',#15264,#15221);
#15226=PRODUCT_DEFINITION('Foot strip (1)','Foot strip (1)',#15265,#15221);
#15227=PRODUCT_DEFINITION('Column cap','Column cap',#15266,#15221);
#15228=PRODUCT_DEFINITION('Rail backing','Rail backing',#15267,#15221);
#15229=PRODUCT_DEFINITION('Travel stop','Travel stop',#15268,#15221);
#15230=PRODUCT_DEFINITION('Travel stop (1)','Travel stop (1)',#15269,#15221);
#15231=PRODUCT_DEFINITION('Spring barrel foot','Spring barrel foot',#15270,
#15221);
#15232=PRODUCT_DEFINITION('Spring barrel','Spring barrel',#15271,#15221);
#15233=PRODUCT_DEFINITION('Rod guide cap','Rod guide cap',#15272,#15221);
#15234=PRODUCT_DEFINITION('Barrel tie stud','Barrel tie stud',#15273,#15221);
#15235=PRODUCT_DEFINITION('M4 top nut','M4 top nut',#15274,#15221);
#15236=PRODUCT_DEFINITION('Barrel tie stud (1)','Barrel tie stud (1)',#15275,
#15221);
#15237=PRODUCT_DEFINITION('M4 top nut (1)','M4 top nut (1)',#15276,#15221);
#15238=PRODUCT_DEFINITION('Installed compression spring',
'Installed compression spring',#15277,#15221);
#15239=PRODUCT_DEFINITION('Column brace','Column brace',#15278,#15221);
#15240=PRODUCT_DEFINITION('Column brace (1)','Column brace (1)',#15279,#15221);
#15241=PRODUCT_DEFINITION('Slotted Extrusion - 20 x 20 x 400 mm',
'Slotted Extrusion - 20 x 20 x 400 mm',#15280,#15221);
#15242=PRODUCT_DEFINITION('Linear Guide Rail - 15 mm, 220 mm Long',
'Linear Guide Rail - 15 mm, 220 mm Long',#15281,#15221);
#15243=PRODUCT_DEFINITION('M5x30 frame screw','M5x30 frame screw',#15282,
#15221);
#15244=PRODUCT_DEFINITION('Cap Screw - M5x20','Cap Screw - M5x20',#15283,
#15221);
#15245=PRODUCT_DEFINITION('Captive slot nut','Captive slot nut',#15284,
#15221);
#15246=PRODUCT_DEFINITION('Flat Washer - M5','Flat Washer - M5',#15285,
#15221);
#15247=PRODUCT_DEFINITION('Moving platform and rod',
'Moving platform and rod',#15286,#15221);
#15248=PRODUCT_DEFINITION('Platform and carriage bracket',
'Platform and carriage bracket',#15287,#15221);
#15249=PRODUCT_DEFINITION('Spring piston','Spring piston',#15288,#15221);
#15250=PRODUCT_DEFINITION('Counterbalance rod','Counterbalance rod',#15289,
#15221);
#15251=PRODUCT_DEFINITION('M10 rod nut','M10 rod nut',#15290,#15221);
#15252=PRODUCT_DEFINITION('Lock bracket','Lock bracket',#15291,#15221);
#15253=PRODUCT_DEFINITION('Retracted lock shoe','Retracted lock shoe',#15292,
#15221);
#15254=PRODUCT_DEFINITION('Lock screw and knob','Lock screw and knob',#15293,
#15221);
#15255=PRODUCT_DEFINITION('Flanged Linear Guide Carriage - 15 mm',
'Flanged Linear Guide Carriage - 15 mm',#15294,#15221);
#15256=PRODUCT_DEFINITION('Block','Block',#15295,#15221);
#15257=PRODUCT_DEFINITION('End cap +','End cap +',#15296,#15221);
#15258=PRODUCT_DEFINITION('End cap','End cap',#15297,#15221);
#15259=PRODUCT_DEFINITION('M5x14 Cap Screw','M5x14 Cap Screw',#15298,#15221);
#15260=PRODUCT_DEFINITION('Cap Screw - M4x16','Cap Screw - M4x16',#15299,
#15221);
#15261=PRODUCT_DEFINITION_FORMATION('',$,#15342);
#15262=PRODUCT_DEFINITION_FORMATION('',$,#15343);
#15263=PRODUCT_DEFINITION_FORMATION('',$,#15344);
#15264=PRODUCT_DEFINITION_FORMATION('',$,#15345);
#15265=PRODUCT_DEFINITION_FORMATION('',$,#15346);
#15266=PRODUCT_DEFINITION_FORMATION('',$,#15347);
#15267=PRODUCT_DEFINITION_FORMATION('',$,#15348);
#15268=PRODUCT_DEFINITION_FORMATION('',$,#15349);
#15269=PRODUCT_DEFINITION_FORMATION('',$,#15350);
#15270=PRODUCT_DEFINITION_FORMATION('',$,#15351);
#15271=PRODUCT_DEFINITION_FORMATION('',$,#15352);
#15272=PRODUCT_DEFINITION_FORMATION('',$,#15353);
#15273=PRODUCT_DEFINITION_FORMATION('',$,#15354);
#15274=PRODUCT_DEFINITION_FORMATION('',$,#15355);
#15275=PRODUCT_DEFINITION_FORMATION('',$,#15356);
#15276=PRODUCT_DEFINITION_FORMATION('',$,#15357);
#15277=PRODUCT_DEFINITION_FORMATION('',$,#15358);
#15278=PRODUCT_DEFINITION_FORMATION('',$,#15359);
#15279=PRODUCT_DEFINITION_FORMATION('',$,#15360);
#15280=PRODUCT_DEFINITION_FORMATION('',$,#15361);
#15281=PRODUCT_DEFINITION_FORMATION('',$,#15362);
#15282=PRODUCT_DEFINITION_FORMATION('',$,#15363);
#15283=PRODUCT_DEFINITION_FORMATION('',$,#15364);
#15284=PRODUCT_DEFINITION_FORMATION('',$,#15365);
#15285=PRODUCT_DEFINITION_FORMATION('',$,#15366);
#15286=PRODUCT_DEFINITION_FORMATION('',$,#15367);
#15287=PRODUCT_DEFINITION_FORMATION('',$,#15368);
#15288=PRODUCT_DEFINITION_FORMATION('',$,#15369);
#15289=PRODUCT_DEFINITION_FORMATION('',$,#15370);
#15290=PRODUCT_DEFINITION_FORMATION('',$,#15371);
#15291=PRODUCT_DEFINITION_FORMATION('',$,#15372);
#15292=PRODUCT_DEFINITION_FORMATION('',$,#15373);
#15293=PRODUCT_DEFINITION_FORMATION('',$,#15374);
#15294=PRODUCT_DEFINITION_FORMATION('',$,#15375);
#15295=PRODUCT_DEFINITION_FORMATION('',$,#15376);
#15296=PRODUCT_DEFINITION_FORMATION('',$,#15377);
#15297=PRODUCT_DEFINITION_FORMATION('',$,#15378);
#15298=PRODUCT_DEFINITION_FORMATION('',$,#15379);
#15299=PRODUCT_DEFINITION_FORMATION('',$,#15380);
#15300=PRODUCT_RELATED_PRODUCT_CATEGORY(
'PAT-117','PAT-117',(#15342));
#15301=PRODUCT_RELATED_PRODUCT_CATEGORY('Column and spring barrel',
'Column and spring barrel',(#15343));
#15302=PRODUCT_RELATED_PRODUCT_CATEGORY('Base foot','Base foot',(#15344));
#15303=PRODUCT_RELATED_PRODUCT_CATEGORY('Foot strip','Foot strip',(#15345));
#15304=PRODUCT_RELATED_PRODUCT_CATEGORY('Foot strip (1)',
'Foot strip (1)',(#15346));
#15305=PRODUCT_RELATED_PRODUCT_CATEGORY('Column cap','Column cap',(#15347));
#15306=PRODUCT_RELATED_PRODUCT_CATEGORY('Rail backing','Rail backing',(#15348));
#15307=PRODUCT_RELATED_PRODUCT_CATEGORY('Travel stop','Travel stop',(#15349));
#15308=PRODUCT_RELATED_PRODUCT_CATEGORY('Travel stop (1)',
'Travel stop (1)',(#15350));
#15309=PRODUCT_RELATED_PRODUCT_CATEGORY('Spring barrel foot',
'Spring barrel foot',(#15351));
#15310=PRODUCT_RELATED_PRODUCT_CATEGORY('Spring barrel','Spring barrel',
(#15352));
#15311=PRODUCT_RELATED_PRODUCT_CATEGORY('Rod guide cap','Rod guide cap',
(#15353));
#15312=PRODUCT_RELATED_PRODUCT_CATEGORY('Barrel tie stud',
'Barrel tie stud',(#15354));
#15313=PRODUCT_RELATED_PRODUCT_CATEGORY('M4 top nut','M4 top nut',(#15355));
#15314=PRODUCT_RELATED_PRODUCT_CATEGORY('Barrel tie stud (1)',
'Barrel tie stud (1)',(#15356));
#15315=PRODUCT_RELATED_PRODUCT_CATEGORY('M4 top nut (1)',
'M4 top nut (1)',(#15357));
#15316=PRODUCT_RELATED_PRODUCT_CATEGORY('Installed compression spring',
'Installed compression spring',(#15358));
#15317=PRODUCT_RELATED_PRODUCT_CATEGORY('Column brace','Column brace',(#15359));
#15318=PRODUCT_RELATED_PRODUCT_CATEGORY('Column brace (1)',
'Column brace (1)',(#15360));
#15319=PRODUCT_RELATED_PRODUCT_CATEGORY(
'Slotted Extrusion - 20 x 20 x 400 mm',
'Slotted Extrusion - 20 x 20 x 400 mm',(#15361));
#15320=PRODUCT_RELATED_PRODUCT_CATEGORY(
'Linear Guide Rail - 15 mm, 220 mm Long',
'Linear Guide Rail - 15 mm, 220 mm Long',(#15362));
#15321=PRODUCT_RELATED_PRODUCT_CATEGORY('M5x30 frame screw',
'M5x30 frame screw',(#15363));
#15322=PRODUCT_RELATED_PRODUCT_CATEGORY('Cap Screw - M5x20',
'Cap Screw - M5x20',(#15364));
#15323=PRODUCT_RELATED_PRODUCT_CATEGORY('Captive slot nut',
'Captive slot nut',(#15365));
#15324=PRODUCT_RELATED_PRODUCT_CATEGORY('Flat Washer - M5',
'Flat Washer - M5',(#15366));
#15325=PRODUCT_RELATED_PRODUCT_CATEGORY('Moving platform and rod',
'Moving platform and rod',(#15367));
#15326=PRODUCT_RELATED_PRODUCT_CATEGORY('Platform and carriage bracket',
'Platform and carriage bracket',(#15368));
#15327=PRODUCT_RELATED_PRODUCT_CATEGORY('Spring piston','Spring piston',
(#15369));
#15328=PRODUCT_RELATED_PRODUCT_CATEGORY('Counterbalance rod',
'Counterbalance rod',(#15370));
#15329=PRODUCT_RELATED_PRODUCT_CATEGORY('M10 rod nut','M10 rod nut',(#15371));
#15330=PRODUCT_RELATED_PRODUCT_CATEGORY('Lock bracket','Lock bracket',(#15372));
#15331=PRODUCT_RELATED_PRODUCT_CATEGORY('Retracted lock shoe',
'Retracted lock shoe',(#15373));
#15332=PRODUCT_RELATED_PRODUCT_CATEGORY('Lock screw and knob',
'Lock screw and knob',(#15374));
#15333=PRODUCT_RELATED_PRODUCT_CATEGORY(
'Flanged Linear Guide Carriage - 15 mm',
'Flanged Linear Guide Carriage - 15 mm',(#15375));
#15334=PRODUCT_RELATED_PRODUCT_CATEGORY('Block','Block',(#15376));
#15335=PRODUCT_RELATED_PRODUCT_CATEGORY('End cap +','End cap +',(#15377));
#15336=PRODUCT_RELATED_PRODUCT_CATEGORY('End cap','End cap',(#15378));
#15337=PRODUCT_RELATED_PRODUCT_CATEGORY('M5x14 Cap Screw',
'M5x14 Cap Screw',(#15379));
#15338=PRODUCT_RELATED_PRODUCT_CATEGORY('Cap Screw - M4x16',
'Cap Screw - M4x16',(#15380));
#15339=APPLICATION_PROTOCOL_DEFINITION('international standard',
'automotive_design',2009,#15340);
#15340=APPLICATION_CONTEXT(
'Core Data for Automotive Mechanical Design Process');
#15341=PRODUCT_CONTEXT('part definition',#15340,'mechanical');
#15342=PRODUCT('PAT-117',
'PAT-117','PAT-117',(#15341));
#15343=PRODUCT('Column and spring barrel','Column and spring barrel',
'Column and spring barrel',(#15341));
#15344=PRODUCT('Base foot','Base foot','Base foot',(#15341));
#15345=PRODUCT('Foot strip','Foot strip','Foot strip',(#15341));
#15346=PRODUCT('Foot strip (1)','Foot strip (1)','Foot strip (1)',(#15341));
#15347=PRODUCT('Column cap','Column cap','Column cap',(#15341));
#15348=PRODUCT('Rail backing','Rail backing','Rail backing',(#15341));
#15349=PRODUCT('Travel stop','Travel stop','Travel stop',(#15341));
#15350=PRODUCT('Travel stop (1)','Travel stop (1)','Travel stop (1)',(#15341));
#15351=PRODUCT('Spring barrel foot','Spring barrel foot',
'Spring barrel foot',(#15341));
#15352=PRODUCT('Spring barrel','Spring barrel','Spring barrel',(#15341));
#15353=PRODUCT('Rod guide cap','Rod guide cap','Rod guide cap',(#15341));
#15354=PRODUCT('Barrel tie stud','Barrel tie stud','Barrel tie stud',(#15341));
#15355=PRODUCT('M4 top nut','M4 top nut','M4 top nut',(#15341));
#15356=PRODUCT('Barrel tie stud (1)','Barrel tie stud (1)',
'Barrel tie stud (1)',(#15341));
#15357=PRODUCT('M4 top nut (1)','M4 top nut (1)','M4 top nut (1)',(#15341));
#15358=PRODUCT('Installed compression spring',
'Installed compression spring','Installed compression spring',(#15341));
#15359=PRODUCT('Column brace','Column brace','Column brace',(#15341));
#15360=PRODUCT('Column brace (1)','Column brace (1)','Column brace (1)',(#15341));
#15361=PRODUCT('Slotted Extrusion - 20 x 20 x 400 mm',
'Slotted Extrusion - 20 x 20 x 400 mm',
'Slotted Extrusion - 20 x 20 x 400 mm',(#15341));
#15362=PRODUCT('Linear Guide Rail - 15 mm, 220 mm Long',
'Linear Guide Rail - 15 mm, 220 mm Long',
'Linear Guide Rail - 15 mm, 220 mm Long',(#15341));
#15363=PRODUCT('M5x30 frame screw','M5x30 frame screw',
'M5x30 frame screw',(#15341));
#15364=PRODUCT('Cap Screw - M5x20','Cap Screw - M5x20',
'Cap Screw - M5x20',(#15341));
#15365=PRODUCT('Captive slot nut','Captive slot nut','Captive slot nut',
(#15341));
#15366=PRODUCT('Flat Washer - M5','Flat Washer - M5','Flat Washer - M5',
(#15341));
#15367=PRODUCT('Moving platform and rod','Moving platform and rod',
'Moving platform and rod',(#15341));
#15368=PRODUCT('Platform and carriage bracket',
'Platform and carriage bracket','Platform and carriage bracket',(#15341));
#15369=PRODUCT('Spring piston','Spring piston','Spring piston',(#15341));
#15370=PRODUCT('Counterbalance rod','Counterbalance rod',
'Counterbalance rod',(#15341));
#15371=PRODUCT('M10 rod nut','M10 rod nut','M10 rod nut',(#15341));
#15372=PRODUCT('Lock bracket','Lock bracket','Lock bracket',(#15341));
#15373=PRODUCT('Retracted lock shoe','Retracted lock shoe',
'Retracted lock shoe',(#15341));
#15374=PRODUCT('Lock screw and knob','Lock screw and knob',
'Lock screw and knob',(#15341));
#15375=PRODUCT('Flanged Linear Guide Carriage - 15 mm',
'Flanged Linear Guide Carriage - 15 mm',
'Flanged Linear Guide Carriage - 15 mm',(#15341));
#15376=PRODUCT('Block','Block','Block',(#15341));
#15377=PRODUCT('End cap +','End cap +','End cap +',(#15341));
#15378=PRODUCT('End cap','End cap','End cap',(#15341));
#15379=PRODUCT('M5x14 Cap Screw','M5x14 Cap Screw','M5x14 Cap Screw',(#15341));
#15380=PRODUCT('Cap Screw - M4x16','Cap Screw - M4x16',
'Cap Screw - M4x16',(#15341));
#15381=PRESENTATION_STYLE_ASSIGNMENT((#15388));
#15382=PRESENTATION_STYLE_ASSIGNMENT((#15389));
#15383=PRESENTATION_STYLE_ASSIGNMENT((#15390));
#15384=PRESENTATION_STYLE_ASSIGNMENT((#15391));
#15385=PRESENTATION_STYLE_ASSIGNMENT((#15392));
#15386=PRESENTATION_STYLE_ASSIGNMENT((#15393));
#15387=PRESENTATION_STYLE_ASSIGNMENT((#15394));
#15388=SURFACE_STYLE_USAGE(.BOTH.,#15395);
#15389=SURFACE_STYLE_USAGE(.BOTH.,#15396);
#15390=SURFACE_STYLE_USAGE(.BOTH.,#15397);
#15391=SURFACE_STYLE_USAGE(.BOTH.,#15398);
#15392=SURFACE_STYLE_USAGE(.BOTH.,#15399);
#15393=SURFACE_STYLE_USAGE(.BOTH.,#15400);
#15394=SURFACE_STYLE_USAGE(.BOTH.,#15401);
#15395=SURFACE_SIDE_STYLE('',(#15402));
#15396=SURFACE_SIDE_STYLE('',(#15403));
#15397=SURFACE_SIDE_STYLE('',(#15404));
#15398=SURFACE_SIDE_STYLE('',(#15405));
#15399=SURFACE_SIDE_STYLE('',(#15406));
#15400=SURFACE_SIDE_STYLE('',(#15407));
#15401=SURFACE_SIDE_STYLE('',(#15408));
#15402=SURFACE_STYLE_FILL_AREA(#15409);
#15403=SURFACE_STYLE_FILL_AREA(#15410);
#15404=SURFACE_STYLE_FILL_AREA(#15411);
#15405=SURFACE_STYLE_FILL_AREA(#15412);
#15406=SURFACE_STYLE_FILL_AREA(#15413);
#15407=SURFACE_STYLE_FILL_AREA(#15414);
#15408=SURFACE_STYLE_FILL_AREA(#15415);
#15409=FILL_AREA_STYLE('Steel - Satin',(#15416));
#15410=FILL_AREA_STYLE('CAD Library Painted - Deep blue',(#15417));
#15411=FILL_AREA_STYLE('CAD Library Painted - Engineering blue',(#15418));
#15412=FILL_AREA_STYLE('CAD Library Painted - Steel gray',(#15419));
#15413=FILL_AREA_STYLE('CAD Library Painted - Off white',(#15420));
#15414=FILL_AREA_STYLE('CAD Library Painted - Graphite',(#15421));
#15415=FILL_AREA_STYLE('CAD Library Painted - Light blue',(#15422));
#15416=FILL_AREA_STYLE_COLOUR('Steel - Satin',#15423);
#15417=FILL_AREA_STYLE_COLOUR('CAD Library Painted - Deep blue',#15424);
#15418=FILL_AREA_STYLE_COLOUR('CAD Library Painted - Engineering blue',
#15425);
#15419=FILL_AREA_STYLE_COLOUR('CAD Library Painted - Steel gray',#15426);
#15420=FILL_AREA_STYLE_COLOUR('CAD Library Painted - Off white',#15427);
#15421=FILL_AREA_STYLE_COLOUR('CAD Library Painted - Graphite',#15428);
#15422=FILL_AREA_STYLE_COLOUR('CAD Library Painted - Light blue',#15429);
#15423=COLOUR_RGB('Steel - Satin',0.627450980392157,0.627450980392157,0.627450980392157);
#15424=COLOUR_RGB('CAD Library Painted - Deep blue',0.0784313725490196,
0.203921568627451,0.349019607843137);
#15425=COLOUR_RGB('CAD Library Painted - Engineering blue',0.12156862745098,
0.356862745098039,0.6);
#15426=COLOUR_RGB('CAD Library Painted - Steel gray',0.592156862745098,
0.631372549019608,0.67843137254902);
#15427=COLOUR_RGB('CAD Library Painted - Off white',0.909803921568627,0.901960784313726,
0.858823529411765);
#15428=COLOUR_RGB('CAD Library Painted - Graphite',0.0980392156862745,0.109803921568627,
0.125490196078431);
#15429=COLOUR_RGB('CAD Library Painted - Light blue',0.286274509803922,
0.552941176470588,0.780392156862745);
#15430=COLOUR_RGB('Dark Blue',0.08,0.2,0.34);
#15431=FILL_AREA_STYLE_COLOUR('',#15430);
#15432=FILL_AREA_STYLE('',(#15431));
#15433=SURFACE_STYLE_FILL_AREA(#15432);
#15434=SURFACE_SIDE_STYLE('',(#15433));
#15435=SURFACE_STYLE_USAGE(.BOTH.,#15434);
#15436=PRESENTATION_STYLE_ASSIGNMENT((#15435));
#15437=COLOUR_RGB('Light Blue',0.38,0.62,0.78);
#15438=FILL_AREA_STYLE_COLOUR('',#15437);
#15439=FILL_AREA_STYLE('',(#15438));
#15440=SURFACE_STYLE_FILL_AREA(#15439);
#15441=SURFACE_SIDE_STYLE('',(#15440));
#15442=SURFACE_STYLE_USAGE(.BOTH.,#15441);
#15443=PRESENTATION_STYLE_ASSIGNMENT((#15442));
#15444=COLOUR_RGB('Sky Blue',0.24,0.69,0.87);
#15445=FILL_AREA_STYLE_COLOUR('',#15444);
#15446=FILL_AREA_STYLE('',(#15445));
#15447=SURFACE_STYLE_FILL_AREA(#15446);
#15448=SURFACE_SIDE_STYLE('',(#15447));
#15449=SURFACE_STYLE_USAGE(.BOTH.,#15448);
#15450=PRESENTATION_STYLE_ASSIGNMENT((#15449));
#15451=COLOUR_RGB('Grey',0.48,0.52,0.57);
#15452=FILL_AREA_STYLE_COLOUR('',#15451);
#15453=FILL_AREA_STYLE('',(#15452));
#15454=SURFACE_STYLE_FILL_AREA(#15453);
#15455=SURFACE_SIDE_STYLE('',(#15454));
#15456=SURFACE_STYLE_USAGE(.BOTH.,#15455);
#15457=PRESENTATION_STYLE_ASSIGNMENT((#15456));
#15458=COLOUR_RGB('Black',0.12,0.14,0.17);
#15459=FILL_AREA_STYLE_COLOUR('',#15458);
#15460=FILL_AREA_STYLE('',(#15459));
#15461=SURFACE_STYLE_FILL_AREA(#15460);
#15462=SURFACE_SIDE_STYLE('',(#15461));
#15463=SURFACE_STYLE_USAGE(.BOTH.,#15462);
#15464=PRESENTATION_STYLE_ASSIGNMENT((#15463));
#15465=COLOUR_RGB('Off White',0.89,0.88,0.83);
#15466=FILL_AREA_STYLE_COLOUR('',#15465);
#15467=FILL_AREA_STYLE('',(#15466));
#15468=SURFACE_STYLE_FILL_AREA(#15467);
#15469=SURFACE_SIDE_STYLE('',(#15468));
#15470=SURFACE_STYLE_USAGE(.BOTH.,#15469);
#15471=PRESENTATION_STYLE_ASSIGNMENT((#15470));
ENDSEC;
END-ISO-10303-21;
